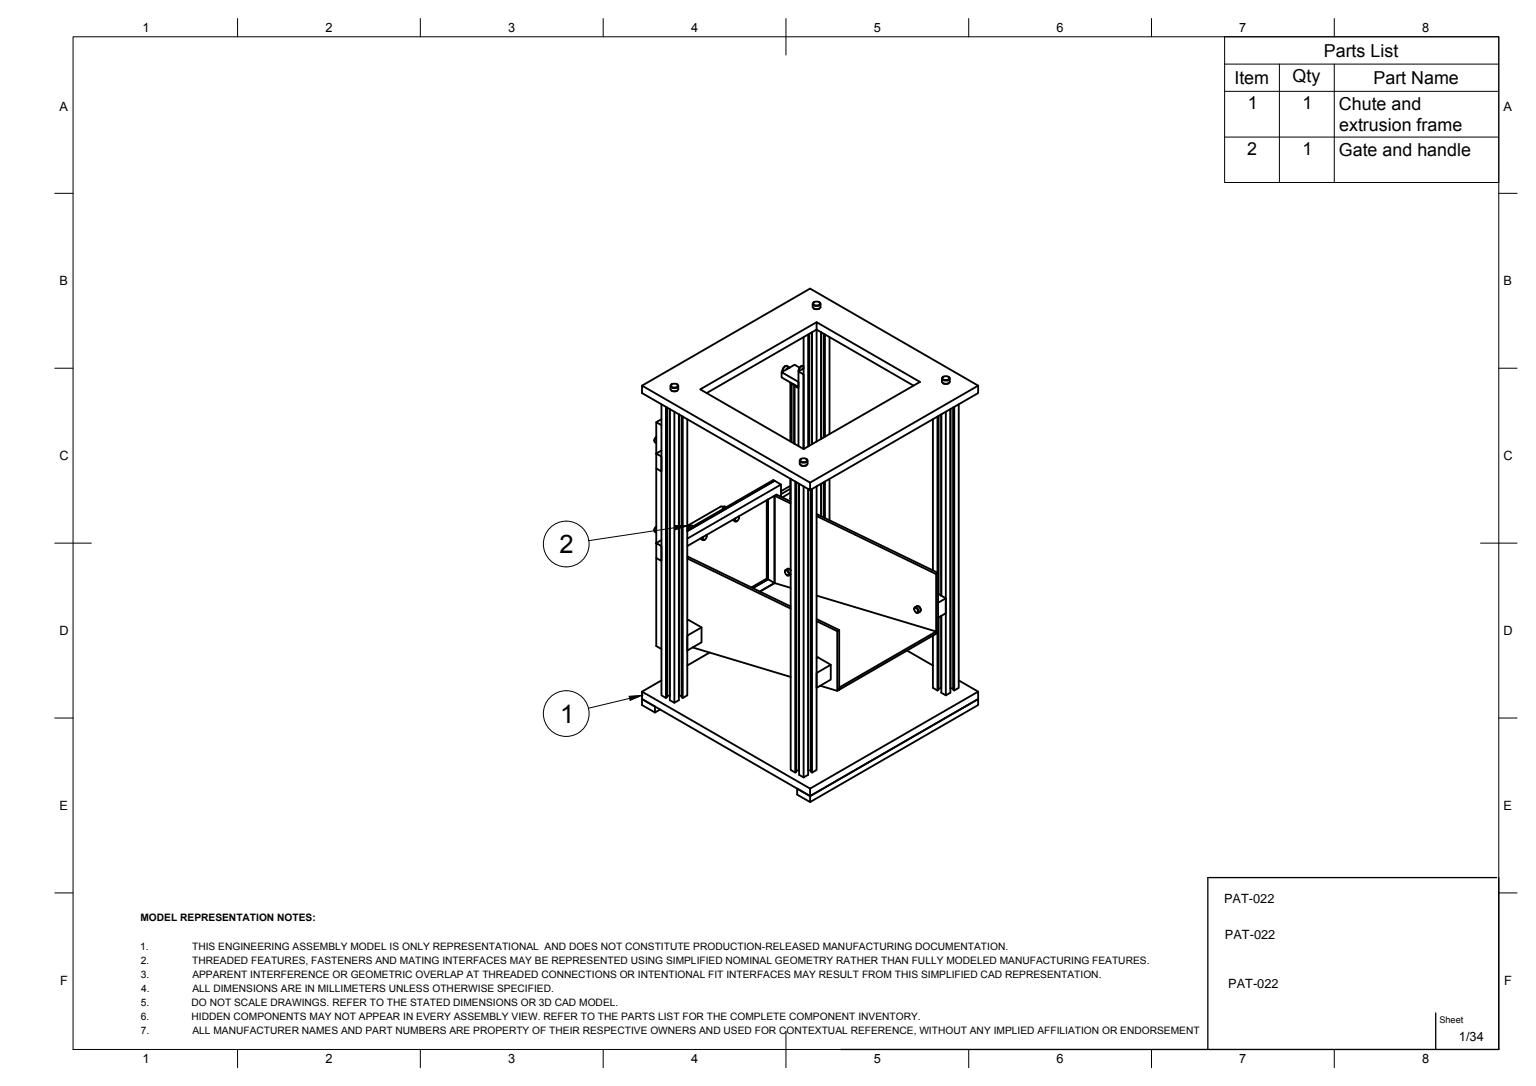
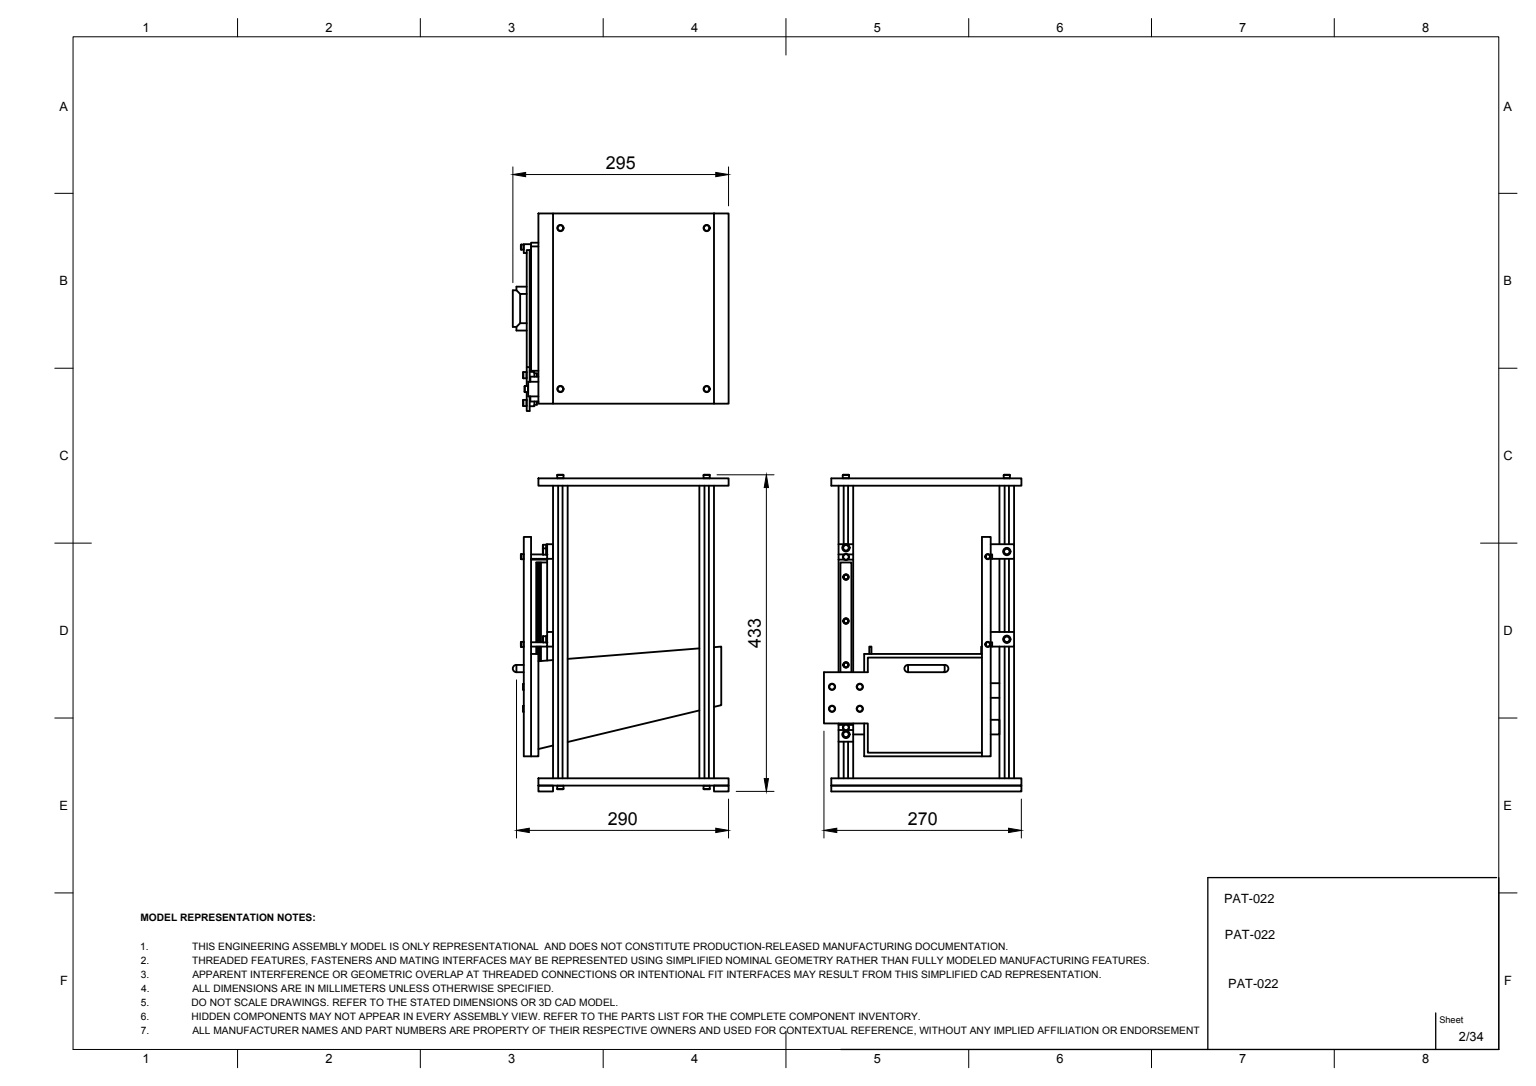
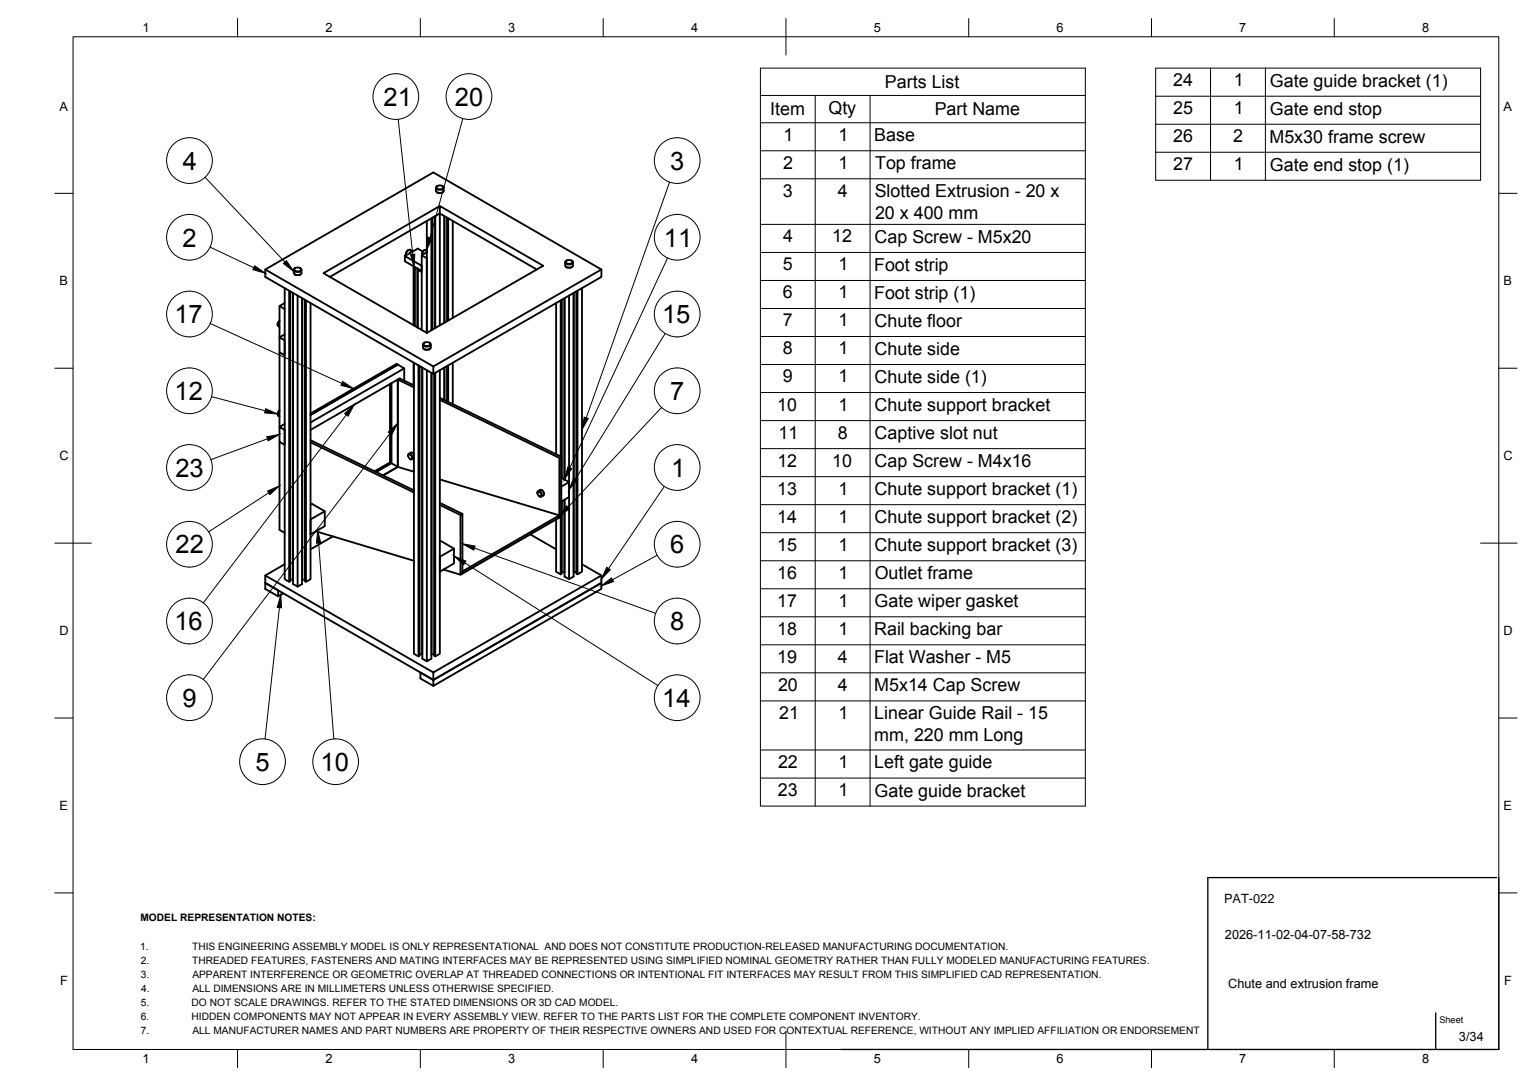
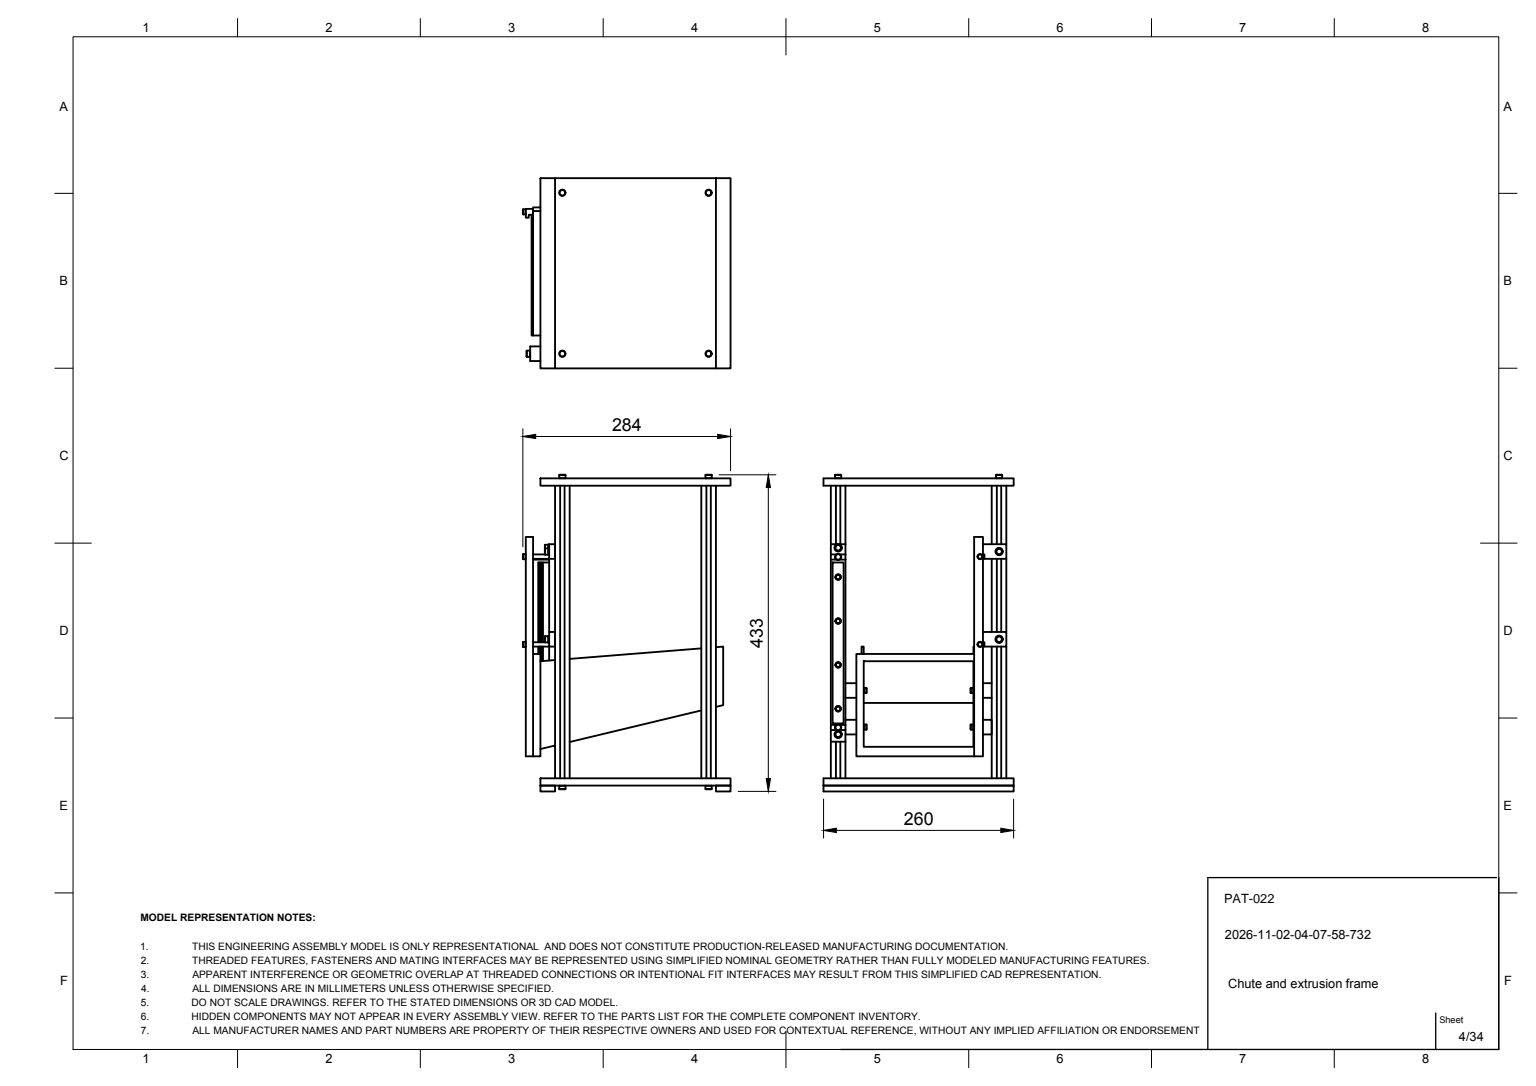
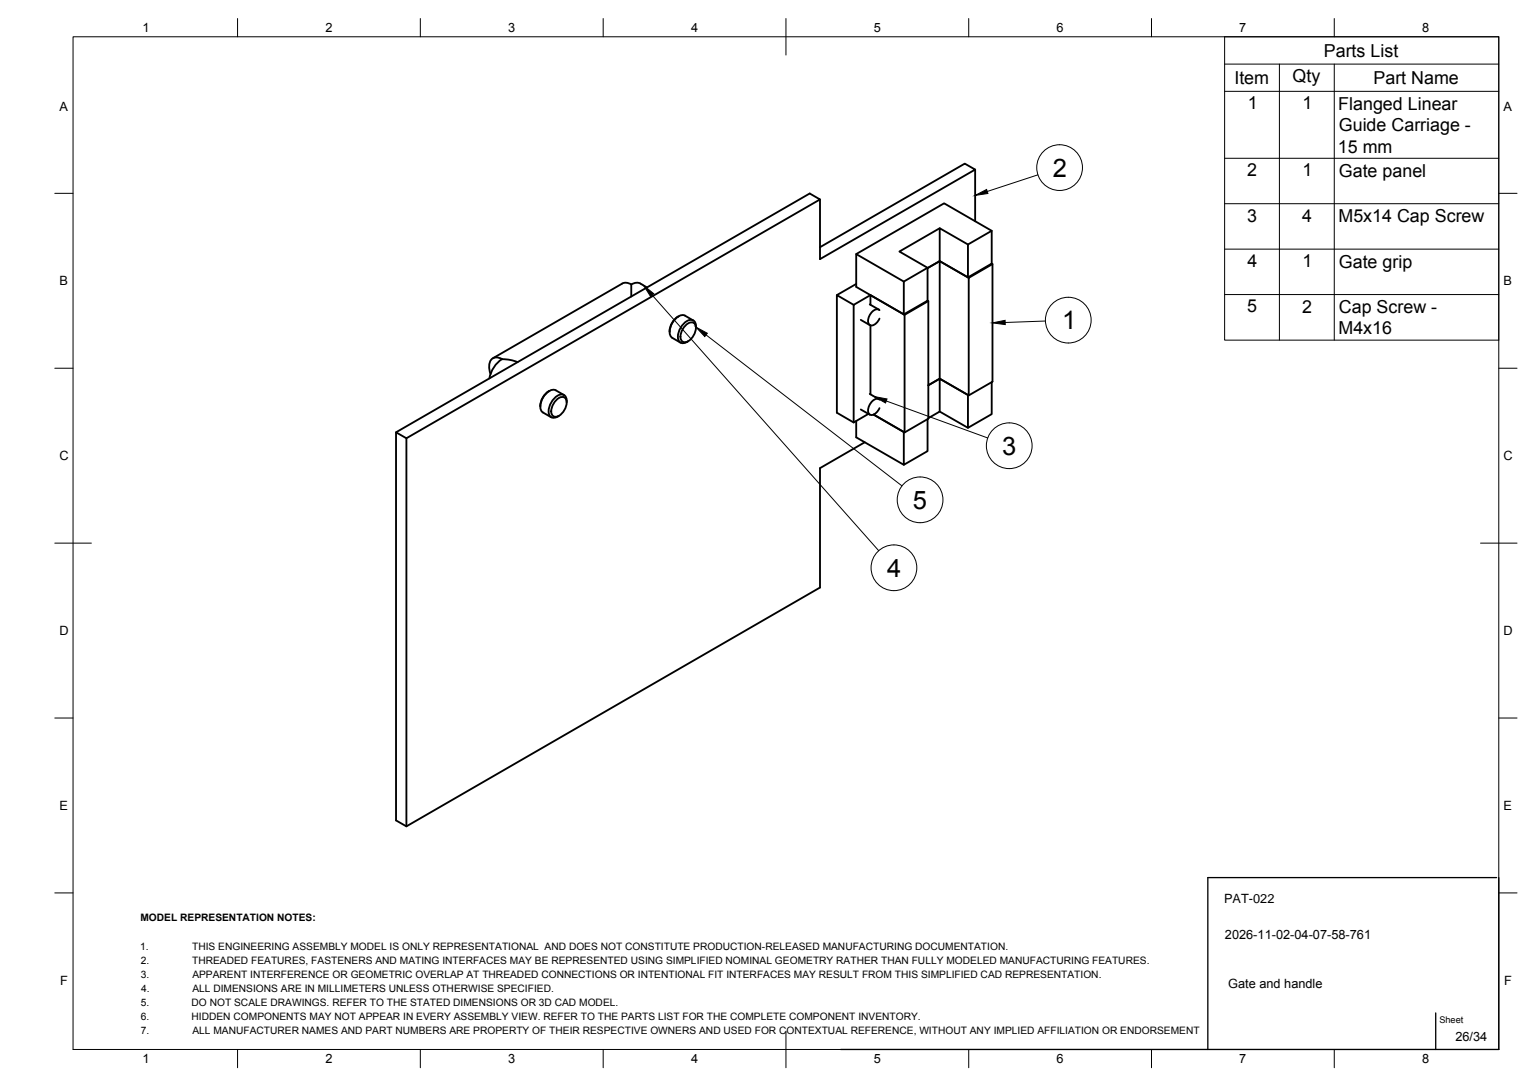
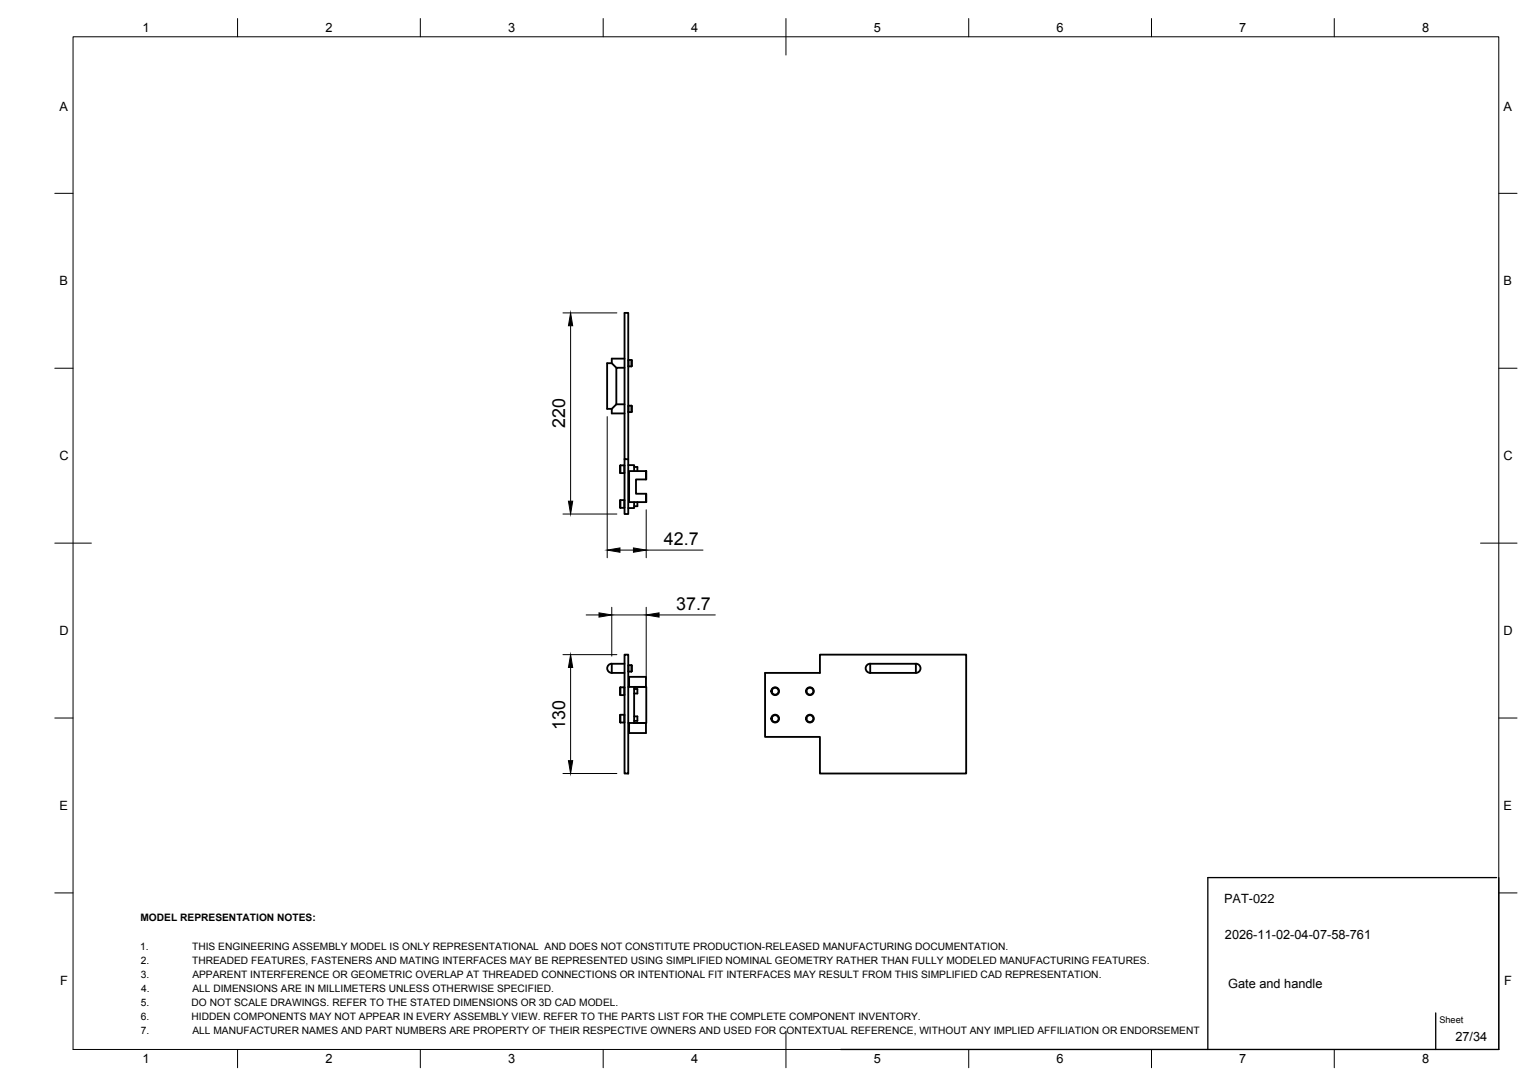
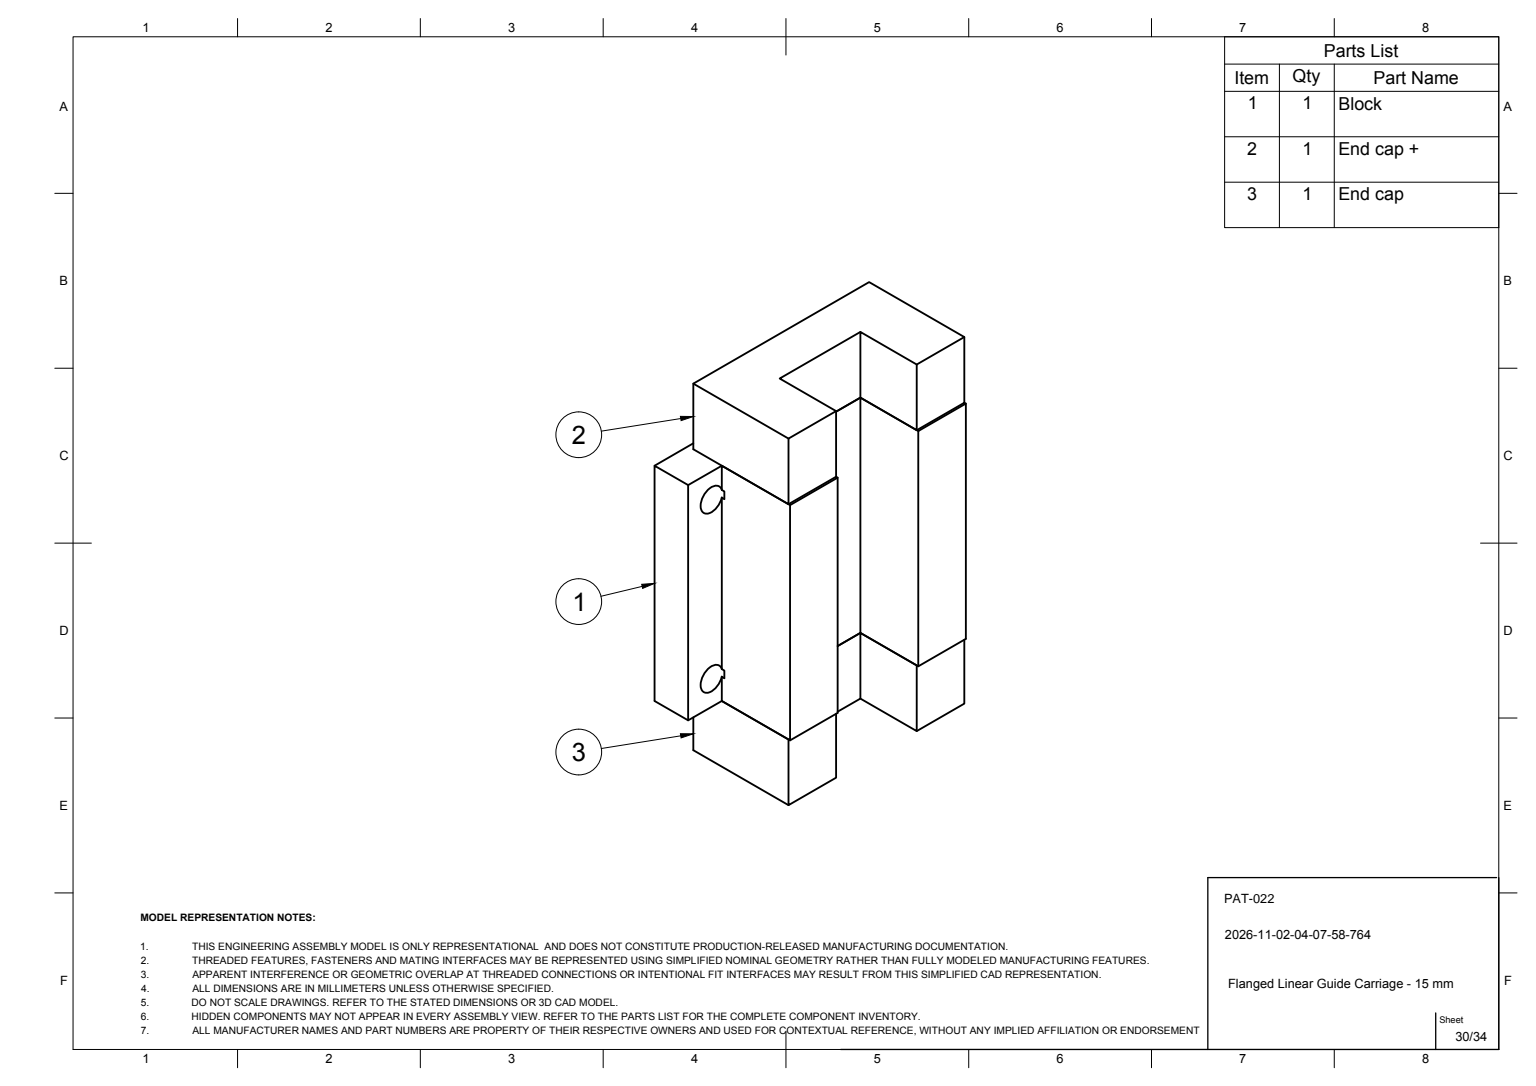
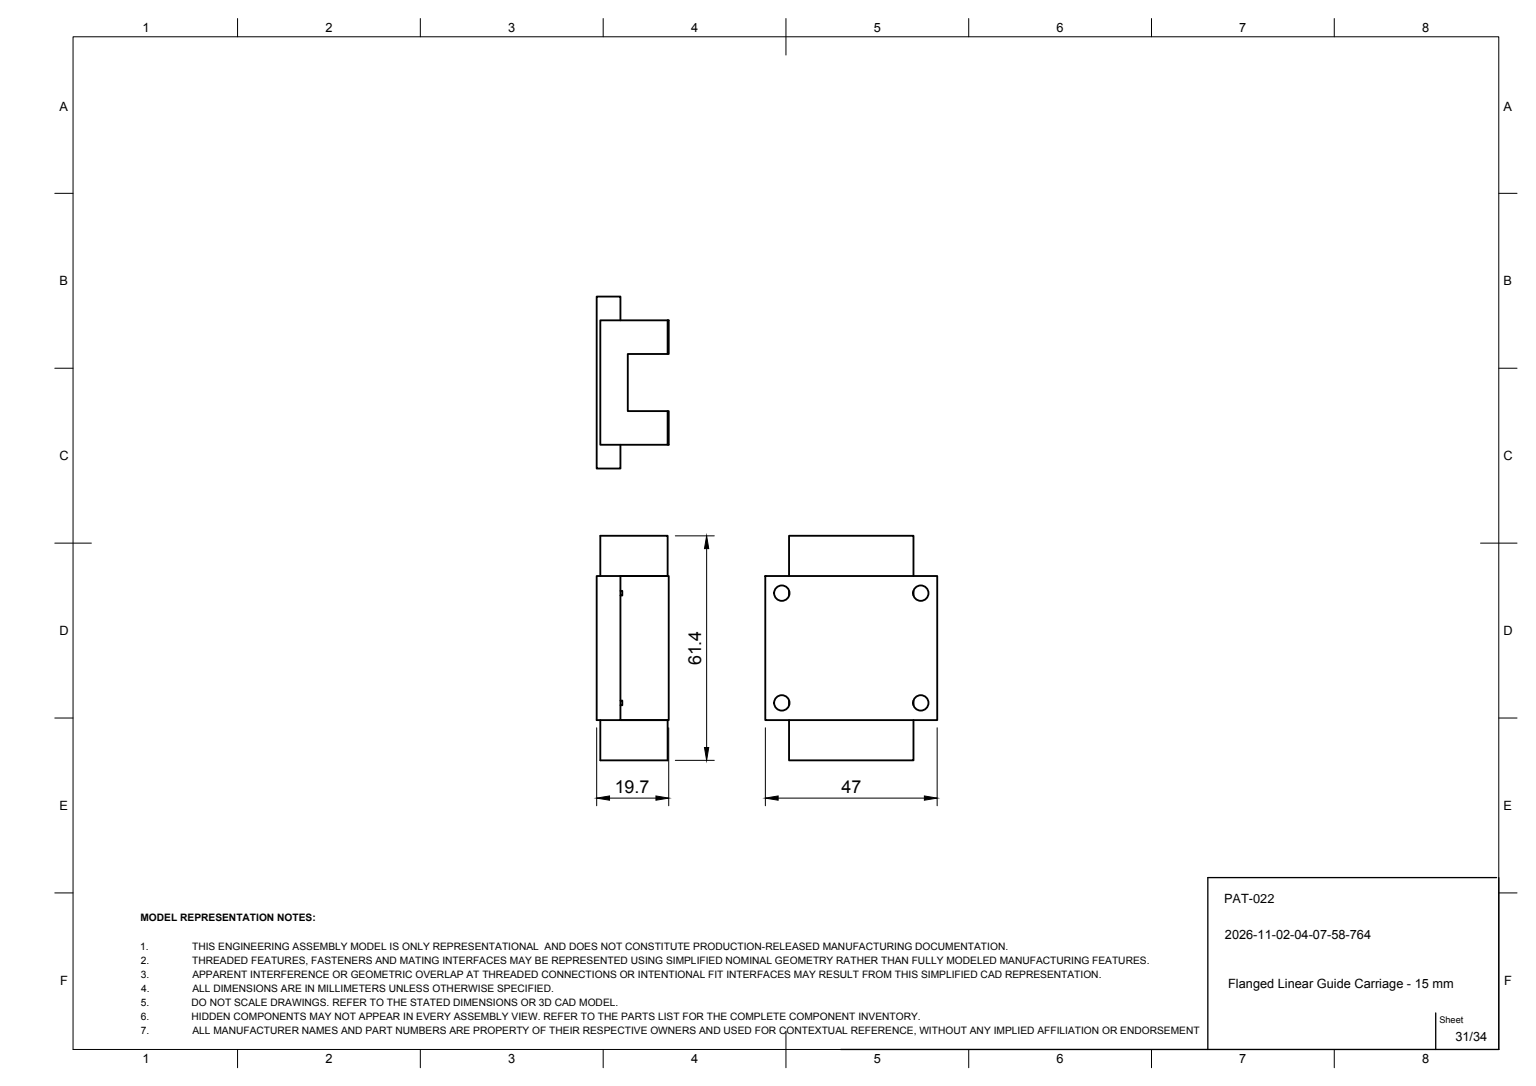
ISO-10303-21;
HEADER;
/* Generated by software containing ST-Developer
 * from STEP Tools, Inc. (www.steptools.com) 
 */

FILE_DESCRIPTION(
/* description */ ('Chute with adjustable gate'),
/* implementation_level */ '2;1');

FILE_NAME(
/* name */ 'PAT-022',
/* time_stamp */ '2026-10-27T10:52:28-07:00',
/* author */ (''),
/* organization */ (''),
/* preprocessor_version */ 'ST-DEVELOPER v20.2',
/* originating_system */ 'Autodesk Translation Framework v15.17.0.0',
/* authorisation */ '');

FILE_SCHEMA (('AUTOMOTIVE_DESIGN { 1 0 10303 214 3 1 1 }'));
ENDSEC;

DATA;
#10=MECHANICAL_DESIGN_GEOMETRIC_PRESENTATION_REPRESENTATION('',(#414,#415,
#416,#417,#418,#419,#420,#421,#422,#423,#424,#425,#426,#427,#428,#429,#430,
#431,#432,#433,#434,#435,#436,#437,#438,#439,#440,#441,#442,#443,#444,#445),
#13094);
#11=ITEM_DEFINED_TRANSFORMATION($,$,#8509,#8570);
#12=ITEM_DEFINED_TRANSFORMATION($,$,#8548,#8571);
#13=ITEM_DEFINED_TRANSFORMATION($,$,#8559,#8572);
#14=ITEM_DEFINED_TRANSFORMATION($,$,#7988,#8623);
#15=ITEM_DEFINED_TRANSFORMATION($,$,#8007,#8624);
#16=ITEM_DEFINED_TRANSFORMATION($,$,#8030,#8625);
#17=ITEM_DEFINED_TRANSFORMATION($,$,#8037,#8626);
#18=ITEM_DEFINED_TRANSFORMATION($,$,#8044,#8627);
#19=ITEM_DEFINED_TRANSFORMATION($,$,#8051,#8628);
#20=ITEM_DEFINED_TRANSFORMATION($,$,#8064,#8629);
#21=ITEM_DEFINED_TRANSFORMATION($,$,#8077,#8630);
#22=ITEM_DEFINED_TRANSFORMATION($,$,#8095,#8631);
#23=ITEM_DEFINED_TRANSFORMATION($,$,#8113,#8632);
#24=ITEM_DEFINED_TRANSFORMATION($,$,#8131,#8633);
#25=ITEM_DEFINED_TRANSFORMATION($,$,#8149,#8634);
#26=ITEM_DEFINED_TRANSFORMATION($,$,#8160,#8635);
#27=ITEM_DEFINED_TRANSFORMATION($,$,#8171,#8636);
#28=ITEM_DEFINED_TRANSFORMATION($,$,#8202,#8637);
#29=ITEM_DEFINED_TRANSFORMATION($,$,#8217,#8638);
#30=ITEM_DEFINED_TRANSFORMATION($,$,#8234,#8639);
#31=ITEM_DEFINED_TRANSFORMATION($,$,#8251,#8640);
#32=ITEM_DEFINED_TRANSFORMATION($,$,#8261,#8641);
#33=ITEM_DEFINED_TRANSFORMATION($,$,#8271,#8642);
#34=ITEM_DEFINED_TRANSFORMATION($,$,#8321,#8643);
#35=ITEM_DEFINED_TRANSFORMATION($,$,#8321,#8644);
#36=ITEM_DEFINED_TRANSFORMATION($,$,#8271,#8645);
#37=ITEM_DEFINED_TRANSFORMATION($,$,#8321,#8646);
#38=ITEM_DEFINED_TRANSFORMATION($,$,#8321,#8647);
#39=ITEM_DEFINED_TRANSFORMATION($,$,#8271,#8648);
#40=ITEM_DEFINED_TRANSFORMATION($,$,#8321,#8649);
#41=ITEM_DEFINED_TRANSFORMATION($,$,#8321,#8650);
#42=ITEM_DEFINED_TRANSFORMATION($,$,#8271,#8651);
#43=ITEM_DEFINED_TRANSFORMATION($,$,#8321,#8652);
#44=ITEM_DEFINED_TRANSFORMATION($,$,#8321,#8653);
#45=ITEM_DEFINED_TRANSFORMATION($,$,#8390,#8654);
#46=ITEM_DEFINED_TRANSFORMATION($,$,#8321,#8655);
#47=ITEM_DEFINED_TRANSFORMATION($,$,#8597,#8656);
#48=ITEM_DEFINED_TRANSFORMATION($,$,#8390,#8657);
#49=ITEM_DEFINED_TRANSFORMATION($,$,#8321,#8658);
#50=ITEM_DEFINED_TRANSFORMATION($,$,#8597,#8659);
#51=ITEM_DEFINED_TRANSFORMATION($,$,#8390,#8660);
#52=ITEM_DEFINED_TRANSFORMATION($,$,#8321,#8661);
#53=ITEM_DEFINED_TRANSFORMATION($,$,#8597,#8662);
#54=ITEM_DEFINED_TRANSFORMATION($,$,#8390,#8663);
#55=ITEM_DEFINED_TRANSFORMATION($,$,#8321,#8664);
#56=ITEM_DEFINED_TRANSFORMATION($,$,#8597,#8665);
#57=ITEM_DEFINED_TRANSFORMATION($,$,#8390,#8666);
#58=ITEM_DEFINED_TRANSFORMATION($,$,#8411,#8667);
#59=ITEM_DEFINED_TRANSFORMATION($,$,#8573,#8668);
#60=ITEM_DEFINED_TRANSFORMATION($,$,#8390,#8669);
#61=ITEM_DEFINED_TRANSFORMATION($,$,#8411,#8670);
#62=ITEM_DEFINED_TRANSFORMATION($,$,#8573,#8671);
#63=ITEM_DEFINED_TRANSFORMATION($,$,#8347,#8672);
#64=ITEM_DEFINED_TRANSFORMATION($,$,#8597,#8673);
#65=ITEM_DEFINED_TRANSFORMATION($,$,#8597,#8674);
#66=ITEM_DEFINED_TRANSFORMATION($,$,#8597,#8675);
#67=ITEM_DEFINED_TRANSFORMATION($,$,#8597,#8676);
#68=ITEM_DEFINED_TRANSFORMATION($,$,#8390,#8677);
#69=ITEM_DEFINED_TRANSFORMATION($,$,#8411,#8678);
#70=ITEM_DEFINED_TRANSFORMATION($,$,#8573,#8679);
#71=ITEM_DEFINED_TRANSFORMATION($,$,#8597,#8680);
#72=ITEM_DEFINED_TRANSFORMATION($,$,#8390,#8681);
#73=ITEM_DEFINED_TRANSFORMATION($,$,#8411,#8682);
#74=ITEM_DEFINED_TRANSFORMATION($,$,#8573,#8683);
#75=ITEM_DEFINED_TRANSFORMATION($,$,#8597,#8684);
#76=ITEM_DEFINED_TRANSFORMATION($,$,#8422,#8685);
#77=ITEM_DEFINED_TRANSFORMATION($,$,#8422,#8686);
#78=ITEM_DEFINED_TRANSFORMATION($,$,#8451,#8687);
#79=ITEM_DEFINED_TRANSFORMATION($,$,#8480,#8688);
#80=ITEM_DEFINED_TRANSFORMATION($,$,#8508,#8689);
#81=ITEM_DEFINED_TRANSFORMATION($,$,#8573,#8690);
#82=ITEM_DEFINED_TRANSFORMATION($,$,#8573,#8691);
#83=ITEM_DEFINED_TRANSFORMATION($,$,#8573,#8692);
#84=ITEM_DEFINED_TRANSFORMATION($,$,#8573,#8693);
#85=ITEM_DEFINED_TRANSFORMATION($,$,#8597,#8694);
#86=ITEM_DEFINED_TRANSFORMATION($,$,#8597,#8695);
#87=ITEM_DEFINED_TRANSFORMATION($,$,#7987,#8696);
#88=ITEM_DEFINED_TRANSFORMATION($,$,#8450,#8697);
#89=(
REPRESENTATION_RELATIONSHIP($,$,#13280,#13279)
REPRESENTATION_RELATIONSHIP_WITH_TRANSFORMATION(#11)
SHAPE_REPRESENTATION_RELATIONSHIP()
);
#90=(
REPRESENTATION_RELATIONSHIP($,$,#13281,#13279)
REPRESENTATION_RELATIONSHIP_WITH_TRANSFORMATION(#12)
SHAPE_REPRESENTATION_RELATIONSHIP()
);
#91=(
REPRESENTATION_RELATIONSHIP($,$,#13282,#13279)
REPRESENTATION_RELATIONSHIP_WITH_TRANSFORMATION(#13)
SHAPE_REPRESENTATION_RELATIONSHIP()
);
#92=(
REPRESENTATION_RELATIONSHIP($,$,#13251,#13250)
REPRESENTATION_RELATIONSHIP_WITH_TRANSFORMATION(#14)
SHAPE_REPRESENTATION_RELATIONSHIP()
);
#93=(
REPRESENTATION_RELATIONSHIP($,$,#13252,#13250)
REPRESENTATION_RELATIONSHIP_WITH_TRANSFORMATION(#15)
SHAPE_REPRESENTATION_RELATIONSHIP()
);
#94=(
REPRESENTATION_RELATIONSHIP($,$,#13253,#13250)
REPRESENTATION_RELATIONSHIP_WITH_TRANSFORMATION(#16)
SHAPE_REPRESENTATION_RELATIONSHIP()
);
#95=(
REPRESENTATION_RELATIONSHIP($,$,#13254,#13250)
REPRESENTATION_RELATIONSHIP_WITH_TRANSFORMATION(#17)
SHAPE_REPRESENTATION_RELATIONSHIP()
);
#96=(
REPRESENTATION_RELATIONSHIP($,$,#13255,#13250)
REPRESENTATION_RELATIONSHIP_WITH_TRANSFORMATION(#18)
SHAPE_REPRESENTATION_RELATIONSHIP()
);
#97=(
REPRESENTATION_RELATIONSHIP($,$,#13256,#13250)
REPRESENTATION_RELATIONSHIP_WITH_TRANSFORMATION(#19)
SHAPE_REPRESENTATION_RELATIONSHIP()
);
#98=(
REPRESENTATION_RELATIONSHIP($,$,#13257,#13250)
REPRESENTATION_RELATIONSHIP_WITH_TRANSFORMATION(#20)
SHAPE_REPRESENTATION_RELATIONSHIP()
);
#99=(
REPRESENTATION_RELATIONSHIP($,$,#13258,#13250)
REPRESENTATION_RELATIONSHIP_WITH_TRANSFORMATION(#21)
SHAPE_REPRESENTATION_RELATIONSHIP()
);
#100=(
REPRESENTATION_RELATIONSHIP($,$,#13259,#13250)
REPRESENTATION_RELATIONSHIP_WITH_TRANSFORMATION(#22)
SHAPE_REPRESENTATION_RELATIONSHIP()
);
#101=(
REPRESENTATION_RELATIONSHIP($,$,#13260,#13250)
REPRESENTATION_RELATIONSHIP_WITH_TRANSFORMATION(#23)
SHAPE_REPRESENTATION_RELATIONSHIP()
);
#102=(
REPRESENTATION_RELATIONSHIP($,$,#13261,#13250)
REPRESENTATION_RELATIONSHIP_WITH_TRANSFORMATION(#24)
SHAPE_REPRESENTATION_RELATIONSHIP()
);
#103=(
REPRESENTATION_RELATIONSHIP($,$,#13262,#13250)
REPRESENTATION_RELATIONSHIP_WITH_TRANSFORMATION(#25)
SHAPE_REPRESENTATION_RELATIONSHIP()
);
#104=(
REPRESENTATION_RELATIONSHIP($,$,#13263,#13250)
REPRESENTATION_RELATIONSHIP_WITH_TRANSFORMATION(#26)
SHAPE_REPRESENTATION_RELATIONSHIP()
);
#105=(
REPRESENTATION_RELATIONSHIP($,$,#13264,#13250)
REPRESENTATION_RELATIONSHIP_WITH_TRANSFORMATION(#27)
SHAPE_REPRESENTATION_RELATIONSHIP()
);
#106=(
REPRESENTATION_RELATIONSHIP($,$,#13265,#13250)
REPRESENTATION_RELATIONSHIP_WITH_TRANSFORMATION(#28)
SHAPE_REPRESENTATION_RELATIONSHIP()
);
#107=(
REPRESENTATION_RELATIONSHIP($,$,#13266,#13250)
REPRESENTATION_RELATIONSHIP_WITH_TRANSFORMATION(#29)
SHAPE_REPRESENTATION_RELATIONSHIP()
);
#108=(
REPRESENTATION_RELATIONSHIP($,$,#13267,#13250)
REPRESENTATION_RELATIONSHIP_WITH_TRANSFORMATION(#30)
SHAPE_REPRESENTATION_RELATIONSHIP()
);
#109=(
REPRESENTATION_RELATIONSHIP($,$,#13268,#13250)
REPRESENTATION_RELATIONSHIP_WITH_TRANSFORMATION(#31)
SHAPE_REPRESENTATION_RELATIONSHIP()
);
#110=(
REPRESENTATION_RELATIONSHIP($,$,#13269,#13250)
REPRESENTATION_RELATIONSHIP_WITH_TRANSFORMATION(#32)
SHAPE_REPRESENTATION_RELATIONSHIP()
);
#111=(
REPRESENTATION_RELATIONSHIP($,$,#13270,#13250)
REPRESENTATION_RELATIONSHIP_WITH_TRANSFORMATION(#33)
SHAPE_REPRESENTATION_RELATIONSHIP()
);
#112=(
REPRESENTATION_RELATIONSHIP($,$,#13271,#13250)
REPRESENTATION_RELATIONSHIP_WITH_TRANSFORMATION(#34)
SHAPE_REPRESENTATION_RELATIONSHIP()
);
#113=(
REPRESENTATION_RELATIONSHIP($,$,#13271,#13250)
REPRESENTATION_RELATIONSHIP_WITH_TRANSFORMATION(#35)
SHAPE_REPRESENTATION_RELATIONSHIP()
);
#114=(
REPRESENTATION_RELATIONSHIP($,$,#13270,#13250)
REPRESENTATION_RELATIONSHIP_WITH_TRANSFORMATION(#36)
SHAPE_REPRESENTATION_RELATIONSHIP()
);
#115=(
REPRESENTATION_RELATIONSHIP($,$,#13271,#13250)
REPRESENTATION_RELATIONSHIP_WITH_TRANSFORMATION(#37)
SHAPE_REPRESENTATION_RELATIONSHIP()
);
#116=(
REPRESENTATION_RELATIONSHIP($,$,#13271,#13250)
REPRESENTATION_RELATIONSHIP_WITH_TRANSFORMATION(#38)
SHAPE_REPRESENTATION_RELATIONSHIP()
);
#117=(
REPRESENTATION_RELATIONSHIP($,$,#13270,#13250)
REPRESENTATION_RELATIONSHIP_WITH_TRANSFORMATION(#39)
SHAPE_REPRESENTATION_RELATIONSHIP()
);
#118=(
REPRESENTATION_RELATIONSHIP($,$,#13271,#13250)
REPRESENTATION_RELATIONSHIP_WITH_TRANSFORMATION(#40)
SHAPE_REPRESENTATION_RELATIONSHIP()
);
#119=(
REPRESENTATION_RELATIONSHIP($,$,#13271,#13250)
REPRESENTATION_RELATIONSHIP_WITH_TRANSFORMATION(#41)
SHAPE_REPRESENTATION_RELATIONSHIP()
);
#120=(
REPRESENTATION_RELATIONSHIP($,$,#13270,#13250)
REPRESENTATION_RELATIONSHIP_WITH_TRANSFORMATION(#42)
SHAPE_REPRESENTATION_RELATIONSHIP()
);
#121=(
REPRESENTATION_RELATIONSHIP($,$,#13271,#13250)
REPRESENTATION_RELATIONSHIP_WITH_TRANSFORMATION(#43)
SHAPE_REPRESENTATION_RELATIONSHIP()
);
#122=(
REPRESENTATION_RELATIONSHIP($,$,#13271,#13250)
REPRESENTATION_RELATIONSHIP_WITH_TRANSFORMATION(#44)
SHAPE_REPRESENTATION_RELATIONSHIP()
);
#123=(
REPRESENTATION_RELATIONSHIP($,$,#13273,#13250)
REPRESENTATION_RELATIONSHIP_WITH_TRANSFORMATION(#45)
SHAPE_REPRESENTATION_RELATIONSHIP()
);
#124=(
REPRESENTATION_RELATIONSHIP($,$,#13271,#13250)
REPRESENTATION_RELATIONSHIP_WITH_TRANSFORMATION(#46)
SHAPE_REPRESENTATION_RELATIONSHIP()
);
#125=(
REPRESENTATION_RELATIONSHIP($,$,#13284,#13250)
REPRESENTATION_RELATIONSHIP_WITH_TRANSFORMATION(#47)
SHAPE_REPRESENTATION_RELATIONSHIP()
);
#126=(
REPRESENTATION_RELATIONSHIP($,$,#13273,#13250)
REPRESENTATION_RELATIONSHIP_WITH_TRANSFORMATION(#48)
SHAPE_REPRESENTATION_RELATIONSHIP()
);
#127=(
REPRESENTATION_RELATIONSHIP($,$,#13271,#13250)
REPRESENTATION_RELATIONSHIP_WITH_TRANSFORMATION(#49)
SHAPE_REPRESENTATION_RELATIONSHIP()
);
#128=(
REPRESENTATION_RELATIONSHIP($,$,#13284,#13250)
REPRESENTATION_RELATIONSHIP_WITH_TRANSFORMATION(#50)
SHAPE_REPRESENTATION_RELATIONSHIP()
);
#129=(
REPRESENTATION_RELATIONSHIP($,$,#13273,#13250)
REPRESENTATION_RELATIONSHIP_WITH_TRANSFORMATION(#51)
SHAPE_REPRESENTATION_RELATIONSHIP()
);
#130=(
REPRESENTATION_RELATIONSHIP($,$,#13271,#13250)
REPRESENTATION_RELATIONSHIP_WITH_TRANSFORMATION(#52)
SHAPE_REPRESENTATION_RELATIONSHIP()
);
#131=(
REPRESENTATION_RELATIONSHIP($,$,#13284,#13250)
REPRESENTATION_RELATIONSHIP_WITH_TRANSFORMATION(#53)
SHAPE_REPRESENTATION_RELATIONSHIP()
);
#132=(
REPRESENTATION_RELATIONSHIP($,$,#13273,#13250)
REPRESENTATION_RELATIONSHIP_WITH_TRANSFORMATION(#54)
SHAPE_REPRESENTATION_RELATIONSHIP()
);
#133=(
REPRESENTATION_RELATIONSHIP($,$,#13271,#13250)
REPRESENTATION_RELATIONSHIP_WITH_TRANSFORMATION(#55)
SHAPE_REPRESENTATION_RELATIONSHIP()
);
#134=(
REPRESENTATION_RELATIONSHIP($,$,#13284,#13250)
REPRESENTATION_RELATIONSHIP_WITH_TRANSFORMATION(#56)
SHAPE_REPRESENTATION_RELATIONSHIP()
);
#135=(
REPRESENTATION_RELATIONSHIP($,$,#13273,#13250)
REPRESENTATION_RELATIONSHIP_WITH_TRANSFORMATION(#57)
SHAPE_REPRESENTATION_RELATIONSHIP()
);
#136=(
REPRESENTATION_RELATIONSHIP($,$,#13274,#13250)
REPRESENTATION_RELATIONSHIP_WITH_TRANSFORMATION(#58)
SHAPE_REPRESENTATION_RELATIONSHIP()
);
#137=(
REPRESENTATION_RELATIONSHIP($,$,#13283,#13250)
REPRESENTATION_RELATIONSHIP_WITH_TRANSFORMATION(#59)
SHAPE_REPRESENTATION_RELATIONSHIP()
);
#138=(
REPRESENTATION_RELATIONSHIP($,$,#13273,#13250)
REPRESENTATION_RELATIONSHIP_WITH_TRANSFORMATION(#60)
SHAPE_REPRESENTATION_RELATIONSHIP()
);
#139=(
REPRESENTATION_RELATIONSHIP($,$,#13274,#13250)
REPRESENTATION_RELATIONSHIP_WITH_TRANSFORMATION(#61)
SHAPE_REPRESENTATION_RELATIONSHIP()
);
#140=(
REPRESENTATION_RELATIONSHIP($,$,#13283,#13250)
REPRESENTATION_RELATIONSHIP_WITH_TRANSFORMATION(#62)
SHAPE_REPRESENTATION_RELATIONSHIP()
);
#141=(
REPRESENTATION_RELATIONSHIP($,$,#13272,#13250)
REPRESENTATION_RELATIONSHIP_WITH_TRANSFORMATION(#63)
SHAPE_REPRESENTATION_RELATIONSHIP()
);
#142=(
REPRESENTATION_RELATIONSHIP($,$,#13284,#13250)
REPRESENTATION_RELATIONSHIP_WITH_TRANSFORMATION(#64)
SHAPE_REPRESENTATION_RELATIONSHIP()
);
#143=(
REPRESENTATION_RELATIONSHIP($,$,#13284,#13250)
REPRESENTATION_RELATIONSHIP_WITH_TRANSFORMATION(#65)
SHAPE_REPRESENTATION_RELATIONSHIP()
);
#144=(
REPRESENTATION_RELATIONSHIP($,$,#13284,#13250)
REPRESENTATION_RELATIONSHIP_WITH_TRANSFORMATION(#66)
SHAPE_REPRESENTATION_RELATIONSHIP()
);
#145=(
REPRESENTATION_RELATIONSHIP($,$,#13284,#13250)
REPRESENTATION_RELATIONSHIP_WITH_TRANSFORMATION(#67)
SHAPE_REPRESENTATION_RELATIONSHIP()
);
#146=(
REPRESENTATION_RELATIONSHIP($,$,#13273,#13250)
REPRESENTATION_RELATIONSHIP_WITH_TRANSFORMATION(#68)
SHAPE_REPRESENTATION_RELATIONSHIP()
);
#147=(
REPRESENTATION_RELATIONSHIP($,$,#13274,#13250)
REPRESENTATION_RELATIONSHIP_WITH_TRANSFORMATION(#69)
SHAPE_REPRESENTATION_RELATIONSHIP()
);
#148=(
REPRESENTATION_RELATIONSHIP($,$,#13283,#13250)
REPRESENTATION_RELATIONSHIP_WITH_TRANSFORMATION(#70)
SHAPE_REPRESENTATION_RELATIONSHIP()
);
#149=(
REPRESENTATION_RELATIONSHIP($,$,#13284,#13250)
REPRESENTATION_RELATIONSHIP_WITH_TRANSFORMATION(#71)
SHAPE_REPRESENTATION_RELATIONSHIP()
);
#150=(
REPRESENTATION_RELATIONSHIP($,$,#13273,#13250)
REPRESENTATION_RELATIONSHIP_WITH_TRANSFORMATION(#72)
SHAPE_REPRESENTATION_RELATIONSHIP()
);
#151=(
REPRESENTATION_RELATIONSHIP($,$,#13274,#13250)
REPRESENTATION_RELATIONSHIP_WITH_TRANSFORMATION(#73)
SHAPE_REPRESENTATION_RELATIONSHIP()
);
#152=(
REPRESENTATION_RELATIONSHIP($,$,#13283,#13250)
REPRESENTATION_RELATIONSHIP_WITH_TRANSFORMATION(#74)
SHAPE_REPRESENTATION_RELATIONSHIP()
);
#153=(
REPRESENTATION_RELATIONSHIP($,$,#13284,#13250)
REPRESENTATION_RELATIONSHIP_WITH_TRANSFORMATION(#75)
SHAPE_REPRESENTATION_RELATIONSHIP()
);
#154=(
REPRESENTATION_RELATIONSHIP($,$,#13275,#13250)
REPRESENTATION_RELATIONSHIP_WITH_TRANSFORMATION(#76)
SHAPE_REPRESENTATION_RELATIONSHIP()
);
#155=(
REPRESENTATION_RELATIONSHIP($,$,#13275,#13250)
REPRESENTATION_RELATIONSHIP_WITH_TRANSFORMATION(#77)
SHAPE_REPRESENTATION_RELATIONSHIP()
);
#156=(
REPRESENTATION_RELATIONSHIP($,$,#13277,#13276)
REPRESENTATION_RELATIONSHIP_WITH_TRANSFORMATION(#78)
SHAPE_REPRESENTATION_RELATIONSHIP()
);
#157=(
REPRESENTATION_RELATIONSHIP($,$,#13278,#13276)
REPRESENTATION_RELATIONSHIP_WITH_TRANSFORMATION(#79)
SHAPE_REPRESENTATION_RELATIONSHIP()
);
#158=(
REPRESENTATION_RELATIONSHIP($,$,#13279,#13276)
REPRESENTATION_RELATIONSHIP_WITH_TRANSFORMATION(#80)
SHAPE_REPRESENTATION_RELATIONSHIP()
);
#159=(
REPRESENTATION_RELATIONSHIP($,$,#13283,#13276)
REPRESENTATION_RELATIONSHIP_WITH_TRANSFORMATION(#81)
SHAPE_REPRESENTATION_RELATIONSHIP()
);
#160=(
REPRESENTATION_RELATIONSHIP($,$,#13283,#13276)
REPRESENTATION_RELATIONSHIP_WITH_TRANSFORMATION(#82)
SHAPE_REPRESENTATION_RELATIONSHIP()
);
#161=(
REPRESENTATION_RELATIONSHIP($,$,#13283,#13276)
REPRESENTATION_RELATIONSHIP_WITH_TRANSFORMATION(#83)
SHAPE_REPRESENTATION_RELATIONSHIP()
);
#162=(
REPRESENTATION_RELATIONSHIP($,$,#13283,#13276)
REPRESENTATION_RELATIONSHIP_WITH_TRANSFORMATION(#84)
SHAPE_REPRESENTATION_RELATIONSHIP()
);
#163=(
REPRESENTATION_RELATIONSHIP($,$,#13284,#13276)
REPRESENTATION_RELATIONSHIP_WITH_TRANSFORMATION(#85)
SHAPE_REPRESENTATION_RELATIONSHIP()
);
#164=(
REPRESENTATION_RELATIONSHIP($,$,#13284,#13276)
REPRESENTATION_RELATIONSHIP_WITH_TRANSFORMATION(#86)
SHAPE_REPRESENTATION_RELATIONSHIP()
);
#165=(
REPRESENTATION_RELATIONSHIP($,$,#13250,#13249)
REPRESENTATION_RELATIONSHIP_WITH_TRANSFORMATION(#87)
SHAPE_REPRESENTATION_RELATIONSHIP()
);
#166=(
REPRESENTATION_RELATIONSHIP($,$,#13276,#13249)
REPRESENTATION_RELATIONSHIP_WITH_TRANSFORMATION(#88)
SHAPE_REPRESENTATION_RELATIONSHIP()
);
#167=CONTEXT_DEPENDENT_SHAPE_REPRESENTATION(#89,#13169);
#168=CONTEXT_DEPENDENT_SHAPE_REPRESENTATION(#90,#13170);
#169=CONTEXT_DEPENDENT_SHAPE_REPRESENTATION(#91,#13171);
#170=CONTEXT_DEPENDENT_SHAPE_REPRESENTATION(#92,#13174);
#171=CONTEXT_DEPENDENT_SHAPE_REPRESENTATION(#93,#13175);
#172=CONTEXT_DEPENDENT_SHAPE_REPRESENTATION(#94,#13176);
#173=CONTEXT_DEPENDENT_SHAPE_REPRESENTATION(#95,#13177);
#174=CONTEXT_DEPENDENT_SHAPE_REPRESENTATION(#96,#13178);
#175=CONTEXT_DEPENDENT_SHAPE_REPRESENTATION(#97,#13179);
#176=CONTEXT_DEPENDENT_SHAPE_REPRESENTATION(#98,#13180);
#177=CONTEXT_DEPENDENT_SHAPE_REPRESENTATION(#99,#13181);
#178=CONTEXT_DEPENDENT_SHAPE_REPRESENTATION(#100,#13182);
#179=CONTEXT_DEPENDENT_SHAPE_REPRESENTATION(#101,#13183);
#180=CONTEXT_DEPENDENT_SHAPE_REPRESENTATION(#102,#13184);
#181=CONTEXT_DEPENDENT_SHAPE_REPRESENTATION(#103,#13185);
#182=CONTEXT_DEPENDENT_SHAPE_REPRESENTATION(#104,#13186);
#183=CONTEXT_DEPENDENT_SHAPE_REPRESENTATION(#105,#13187);
#184=CONTEXT_DEPENDENT_SHAPE_REPRESENTATION(#106,#13188);
#185=CONTEXT_DEPENDENT_SHAPE_REPRESENTATION(#107,#13189);
#186=CONTEXT_DEPENDENT_SHAPE_REPRESENTATION(#108,#13190);
#187=CONTEXT_DEPENDENT_SHAPE_REPRESENTATION(#109,#13191);
#188=CONTEXT_DEPENDENT_SHAPE_REPRESENTATION(#110,#13192);
#189=CONTEXT_DEPENDENT_SHAPE_REPRESENTATION(#111,#13193);
#190=CONTEXT_DEPENDENT_SHAPE_REPRESENTATION(#112,#13194);
#191=CONTEXT_DEPENDENT_SHAPE_REPRESENTATION(#113,#13195);
#192=CONTEXT_DEPENDENT_SHAPE_REPRESENTATION(#114,#13196);
#193=CONTEXT_DEPENDENT_SHAPE_REPRESENTATION(#115,#13197);
#194=CONTEXT_DEPENDENT_SHAPE_REPRESENTATION(#116,#13198);
#195=CONTEXT_DEPENDENT_SHAPE_REPRESENTATION(#117,#13199);
#196=CONTEXT_DEPENDENT_SHAPE_REPRESENTATION(#118,#13200);
#197=CONTEXT_DEPENDENT_SHAPE_REPRESENTATION(#119,#13201);
#198=CONTEXT_DEPENDENT_SHAPE_REPRESENTATION(#120,#13202);
#199=CONTEXT_DEPENDENT_SHAPE_REPRESENTATION(#121,#13203);
#200=CONTEXT_DEPENDENT_SHAPE_REPRESENTATION(#122,#13204);
#201=CONTEXT_DEPENDENT_SHAPE_REPRESENTATION(#123,#13205);
#202=CONTEXT_DEPENDENT_SHAPE_REPRESENTATION(#124,#13206);
#203=CONTEXT_DEPENDENT_SHAPE_REPRESENTATION(#125,#13207);
#204=CONTEXT_DEPENDENT_SHAPE_REPRESENTATION(#126,#13208);
#205=CONTEXT_DEPENDENT_SHAPE_REPRESENTATION(#127,#13209);
#206=CONTEXT_DEPENDENT_SHAPE_REPRESENTATION(#128,#13210);
#207=CONTEXT_DEPENDENT_SHAPE_REPRESENTATION(#129,#13211);
#208=CONTEXT_DEPENDENT_SHAPE_REPRESENTATION(#130,#13212);
#209=CONTEXT_DEPENDENT_SHAPE_REPRESENTATION(#131,#13213);
#210=CONTEXT_DEPENDENT_SHAPE_REPRESENTATION(#132,#13214);
#211=CONTEXT_DEPENDENT_SHAPE_REPRESENTATION(#133,#13215);
#212=CONTEXT_DEPENDENT_SHAPE_REPRESENTATION(#134,#13216);
#213=CONTEXT_DEPENDENT_SHAPE_REPRESENTATION(#135,#13217);
#214=CONTEXT_DEPENDENT_SHAPE_REPRESENTATION(#136,#13218);
#215=CONTEXT_DEPENDENT_SHAPE_REPRESENTATION(#137,#13219);
#216=CONTEXT_DEPENDENT_SHAPE_REPRESENTATION(#138,#13220);
#217=CONTEXT_DEPENDENT_SHAPE_REPRESENTATION(#139,#13221);
#218=CONTEXT_DEPENDENT_SHAPE_REPRESENTATION(#140,#13222);
#219=CONTEXT_DEPENDENT_SHAPE_REPRESENTATION(#141,#13223);
#220=CONTEXT_DEPENDENT_SHAPE_REPRESENTATION(#142,#13224);
#221=CONTEXT_DEPENDENT_SHAPE_REPRESENTATION(#143,#13225);
#222=CONTEXT_DEPENDENT_SHAPE_REPRESENTATION(#144,#13226);
#223=CONTEXT_DEPENDENT_SHAPE_REPRESENTATION(#145,#13227);
#224=CONTEXT_DEPENDENT_SHAPE_REPRESENTATION(#146,#13228);
#225=CONTEXT_DEPENDENT_SHAPE_REPRESENTATION(#147,#13229);
#226=CONTEXT_DEPENDENT_SHAPE_REPRESENTATION(#148,#13230);
#227=CONTEXT_DEPENDENT_SHAPE_REPRESENTATION(#149,#13231);
#228=CONTEXT_DEPENDENT_SHAPE_REPRESENTATION(#150,#13232);
#229=CONTEXT_DEPENDENT_SHAPE_REPRESENTATION(#151,#13233);
#230=CONTEXT_DEPENDENT_SHAPE_REPRESENTATION(#152,#13234);
#231=CONTEXT_DEPENDENT_SHAPE_REPRESENTATION(#153,#13235);
#232=CONTEXT_DEPENDENT_SHAPE_REPRESENTATION(#154,#13236);
#233=CONTEXT_DEPENDENT_SHAPE_REPRESENTATION(#155,#13237);
#234=CONTEXT_DEPENDENT_SHAPE_REPRESENTATION(#156,#13238);
#235=CONTEXT_DEPENDENT_SHAPE_REPRESENTATION(#157,#13239);
#236=CONTEXT_DEPENDENT_SHAPE_REPRESENTATION(#158,#13240);
#237=CONTEXT_DEPENDENT_SHAPE_REPRESENTATION(#159,#13241);
#238=CONTEXT_DEPENDENT_SHAPE_REPRESENTATION(#160,#13242);
#239=CONTEXT_DEPENDENT_SHAPE_REPRESENTATION(#161,#13243);
#240=CONTEXT_DEPENDENT_SHAPE_REPRESENTATION(#162,#13244);
#241=CONTEXT_DEPENDENT_SHAPE_REPRESENTATION(#163,#13245);
#242=CONTEXT_DEPENDENT_SHAPE_REPRESENTATION(#164,#13246);
#243=CONTEXT_DEPENDENT_SHAPE_REPRESENTATION(#165,#13247);
#244=CONTEXT_DEPENDENT_SHAPE_REPRESENTATION(#166,#13248);
#245=NEXT_ASSEMBLY_USAGE_OCCURRENCE('Block:1','Block:1','Block:1',#13316,
#13317,'Block:1');
#246=NEXT_ASSEMBLY_USAGE_OCCURRENCE('End cap +:1','End cap +:1',
'End cap +:1',#13316,#13318,'End cap +:1');
#247=NEXT_ASSEMBLY_USAGE_OCCURRENCE('End cap:1','End cap:1','End cap:1',
#13316,#13319,'End cap:1');
#248=NEXT_ASSEMBLY_USAGE_OCCURRENCE('Base:1','Base:1','Base:1',#13287,#13288,
'Base:1');
#249=NEXT_ASSEMBLY_USAGE_OCCURRENCE('Top frame:1','Top frame:1',
'Top frame:1',#13287,#13289,'Top frame:1');
#250=NEXT_ASSEMBLY_USAGE_OCCURRENCE('Foot strip:1','Foot strip:1',
'Foot strip:1',#13287,#13290,'Foot strip:1');
#251=NEXT_ASSEMBLY_USAGE_OCCURRENCE('Foot strip (1):1',
'Foot strip (1):1','Foot strip (1):1',#13287,#13291,'Foot strip (1):1');
#252=NEXT_ASSEMBLY_USAGE_OCCURRENCE('Chute floor:1','Chute floor:1',
'Chute floor:1',#13287,#13292,'Chute floor:1');
#253=NEXT_ASSEMBLY_USAGE_OCCURRENCE('Chute side:1','Chute side:1',
'Chute side:1',#13287,#13293,'Chute side:1');
#254=NEXT_ASSEMBLY_USAGE_OCCURRENCE('Chute side (1):1',
'Chute side (1):1','Chute side (1):1',#13287,#13294,'Chute side (1):1');
#255=NEXT_ASSEMBLY_USAGE_OCCURRENCE('Chute support bracket:1',
'Chute support bracket:1','Chute support bracket:1',#13287,#13295,
'Chute support bracket:1');
#256=NEXT_ASSEMBLY_USAGE_OCCURRENCE('Chute support bracket (1):1',
'Chute support bracket (1):1','Chute support bracket (1):1',#13287,#13296,
'Chute support bracket (1):1');
#257=NEXT_ASSEMBLY_USAGE_OCCURRENCE('Chute support bracket (2):1',
'Chute support bracket (2):1','Chute support bracket (2):1',#13287,#13297,
'Chute support bracket (2):1');
#258=NEXT_ASSEMBLY_USAGE_OCCURRENCE('Chute support bracket (3):1',
'Chute support bracket (3):1','Chute support bracket (3):1',#13287,#13298,
'Chute support bracket (3):1');
#259=NEXT_ASSEMBLY_USAGE_OCCURRENCE('Outlet frame:1','Outlet frame:1',
'Outlet frame:1',#13287,#13299,'Outlet frame:1');
#260=NEXT_ASSEMBLY_USAGE_OCCURRENCE('Gate wiper gasket:1',
'Gate wiper gasket:1','Gate wiper gasket:1',#13287,#13300,
'Gate wiper gasket:1');
#261=NEXT_ASSEMBLY_USAGE_OCCURRENCE('Rail backing bar:1',
'Rail backing bar:1','Rail backing bar:1',#13287,#13301,
'Rail backing bar:1');
#262=NEXT_ASSEMBLY_USAGE_OCCURRENCE('Left gate guide:1',
'Left gate guide:1','Left gate guide:1',#13287,#13302,
'Left gate guide:1');
#263=NEXT_ASSEMBLY_USAGE_OCCURRENCE('Gate guide bracket:1',
'Gate guide bracket:1','Gate guide bracket:1',#13287,#13303,
'Gate guide bracket:1');
#264=NEXT_ASSEMBLY_USAGE_OCCURRENCE('Gate guide bracket (1):1',
'Gate guide bracket (1):1','Gate guide bracket (1):1',#13287,#13304,
'Gate guide bracket (1):1');
#265=NEXT_ASSEMBLY_USAGE_OCCURRENCE('Gate end stop:1','Gate end stop:1',
'Gate end stop:1',#13287,#13305,'Gate end stop:1');
#266=NEXT_ASSEMBLY_USAGE_OCCURRENCE('Gate end stop (1):1',
'Gate end stop (1):1','Gate end stop (1):1',#13287,#13306,
'Gate end stop (1):1');
#267=NEXT_ASSEMBLY_USAGE_OCCURRENCE(
'Slotted Extrusion - 20 x 20 x 400 mm:2',
'Slotted Extrusion - 20 x 20 x 400 mm:2',
'Slotted Extrusion - 20 x 20 x 400 mm:2',#13287,#13307,
'Slotted Extrusion - 20 x 20 x 400 mm:2');
#268=NEXT_ASSEMBLY_USAGE_OCCURRENCE('Cap Screw - M5x20:2',
'Cap Screw - M5x20:2','Cap Screw - M5x20:2',#13287,#13308,
'Cap Screw - M5x20:2');
#269=NEXT_ASSEMBLY_USAGE_OCCURRENCE('Cap Screw - M5x20:3',
'Cap Screw - M5x20:3','Cap Screw - M5x20:3',#13287,#13308,
'Cap Screw - M5x20:3');
#270=NEXT_ASSEMBLY_USAGE_OCCURRENCE(
'Slotted Extrusion - 20 x 20 x 400 mm:3',
'Slotted Extrusion - 20 x 20 x 400 mm:3',
'Slotted Extrusion - 20 x 20 x 400 mm:3',#13287,#13307,
'Slotted Extrusion - 20 x 20 x 400 mm:3');
#271=NEXT_ASSEMBLY_USAGE_OCCURRENCE('Cap Screw - M5x20:4',
'Cap Screw - M5x20:4','Cap Screw - M5x20:4',#13287,#13308,
'Cap Screw - M5x20:4');
#272=NEXT_ASSEMBLY_USAGE_OCCURRENCE('Cap Screw - M5x20:5',
'Cap Screw - M5x20:5','Cap Screw - M5x20:5',#13287,#13308,
'Cap Screw - M5x20:5');
#273=NEXT_ASSEMBLY_USAGE_OCCURRENCE(
'Slotted Extrusion - 20 x 20 x 400 mm:4',
'Slotted Extrusion - 20 x 20 x 400 mm:4',
'Slotted Extrusion - 20 x 20 x 400 mm:4',#13287,#13307,
'Slotted Extrusion - 20 x 20 x 400 mm:4');
#274=NEXT_ASSEMBLY_USAGE_OCCURRENCE('Cap Screw - M5x20:6',
'Cap Screw - M5x20:6','Cap Screw - M5x20:6',#13287,#13308,
'Cap Screw - M5x20:6');
#275=NEXT_ASSEMBLY_USAGE_OCCURRENCE('Cap Screw - M5x20:7',
'Cap Screw - M5x20:7','Cap Screw - M5x20:7',#13287,#13308,
'Cap Screw - M5x20:7');
#276=NEXT_ASSEMBLY_USAGE_OCCURRENCE(
'Slotted Extrusion - 20 x 20 x 400 mm:5',
'Slotted Extrusion - 20 x 20 x 400 mm:5',
'Slotted Extrusion - 20 x 20 x 400 mm:5',#13287,#13307,
'Slotted Extrusion - 20 x 20 x 400 mm:5');
#277=NEXT_ASSEMBLY_USAGE_OCCURRENCE('Cap Screw - M5x20:8',
'Cap Screw - M5x20:8','Cap Screw - M5x20:8',#13287,#13308,
'Cap Screw - M5x20:8');
#278=NEXT_ASSEMBLY_USAGE_OCCURRENCE('Cap Screw - M5x20:9',
'Cap Screw - M5x20:9','Cap Screw - M5x20:9',#13287,#13308,
'Cap Screw - M5x20:9');
#279=NEXT_ASSEMBLY_USAGE_OCCURRENCE('Captive slot nut:2',
'Captive slot nut:2','Captive slot nut:2',#13287,#13310,
'Captive slot nut:2');
#280=NEXT_ASSEMBLY_USAGE_OCCURRENCE('Cap Screw - M5x20:10',
'Cap Screw - M5x20:10','Cap Screw - M5x20:10',#13287,#13308,
'Cap Screw - M5x20:10');
#281=NEXT_ASSEMBLY_USAGE_OCCURRENCE('Cap Screw - M4x16:2',
'Cap Screw - M4x16:2','Cap Screw - M4x16:2',#13287,#13321,
'Cap Screw - M4x16:2');
#282=NEXT_ASSEMBLY_USAGE_OCCURRENCE('Captive slot nut:3',
'Captive slot nut:3','Captive slot nut:3',#13287,#13310,
'Captive slot nut:3');
#283=NEXT_ASSEMBLY_USAGE_OCCURRENCE('Cap Screw - M5x20:11',
'Cap Screw - M5x20:11','Cap Screw - M5x20:11',#13287,#13308,
'Cap Screw - M5x20:11');
#284=NEXT_ASSEMBLY_USAGE_OCCURRENCE('Cap Screw - M4x16:3',
'Cap Screw - M4x16:3','Cap Screw - M4x16:3',#13287,#13321,
'Cap Screw - M4x16:3');
#285=NEXT_ASSEMBLY_USAGE_OCCURRENCE('Captive slot nut:4',
'Captive slot nut:4','Captive slot nut:4',#13287,#13310,
'Captive slot nut:4');
#286=NEXT_ASSEMBLY_USAGE_OCCURRENCE('Cap Screw - M5x20:12',
'Cap Screw - M5x20:12','Cap Screw - M5x20:12',#13287,#13308,
'Cap Screw - M5x20:12');
#287=NEXT_ASSEMBLY_USAGE_OCCURRENCE('Cap Screw - M4x16:4',
'Cap Screw - M4x16:4','Cap Screw - M4x16:4',#13287,#13321,
'Cap Screw - M4x16:4');
#288=NEXT_ASSEMBLY_USAGE_OCCURRENCE('Captive slot nut:5',
'Captive slot nut:5','Captive slot nut:5',#13287,#13310,
'Captive slot nut:5');
#289=NEXT_ASSEMBLY_USAGE_OCCURRENCE('Cap Screw - M5x20:13',
'Cap Screw - M5x20:13','Cap Screw - M5x20:13',#13287,#13308,
'Cap Screw - M5x20:13');
#290=NEXT_ASSEMBLY_USAGE_OCCURRENCE('Cap Screw - M4x16:5',
'Cap Screw - M4x16:5','Cap Screw - M4x16:5',#13287,#13321,
'Cap Screw - M4x16:5');
#291=NEXT_ASSEMBLY_USAGE_OCCURRENCE('Captive slot nut:6',
'Captive slot nut:6','Captive slot nut:6',#13287,#13310,
'Captive slot nut:6');
#292=NEXT_ASSEMBLY_USAGE_OCCURRENCE('Flat Washer - M5:2',
'Flat Washer - M5:2','Flat Washer - M5:2',#13287,#13311,
'Flat Washer - M5:2');
#293=NEXT_ASSEMBLY_USAGE_OCCURRENCE('M5x14 Cap Screw:2',
'M5x14 Cap Screw:2','M5x14 Cap Screw:2',#13287,#13320,
'M5x14 Cap Screw:2');
#294=NEXT_ASSEMBLY_USAGE_OCCURRENCE('Captive slot nut:7',
'Captive slot nut:7','Captive slot nut:7',#13287,#13310,
'Captive slot nut:7');
#295=NEXT_ASSEMBLY_USAGE_OCCURRENCE('Flat Washer - M5:3',
'Flat Washer - M5:3','Flat Washer - M5:3',#13287,#13311,
'Flat Washer - M5:3');
#296=NEXT_ASSEMBLY_USAGE_OCCURRENCE('M5x14 Cap Screw:3',
'M5x14 Cap Screw:3','M5x14 Cap Screw:3',#13287,#13320,
'M5x14 Cap Screw:3');
#297=NEXT_ASSEMBLY_USAGE_OCCURRENCE(
'Linear Guide Rail - 15 mm, 220 mm Long:2',
'Linear Guide Rail - 15 mm, 220 mm Long:2',
'Linear Guide Rail - 15 mm, 220 mm Long:2',#13287,#13309,
'Linear Guide Rail - 15 mm, 220 mm Long:2');
#298=NEXT_ASSEMBLY_USAGE_OCCURRENCE('Cap Screw - M4x16:6',
'Cap Screw - M4x16:6','Cap Screw - M4x16:6',#13287,#13321,
'Cap Screw - M4x16:6');
#299=NEXT_ASSEMBLY_USAGE_OCCURRENCE('Cap Screw - M4x16:7',
'Cap Screw - M4x16:7','Cap Screw - M4x16:7',#13287,#13321,
'Cap Screw - M4x16:7');
#300=NEXT_ASSEMBLY_USAGE_OCCURRENCE('Cap Screw - M4x16:8',
'Cap Screw - M4x16:8','Cap Screw - M4x16:8',#13287,#13321,
'Cap Screw - M4x16:8');
#301=NEXT_ASSEMBLY_USAGE_OCCURRENCE('Cap Screw - M4x16:9',
'Cap Screw - M4x16:9','Cap Screw - M4x16:9',#13287,#13321,
'Cap Screw - M4x16:9');
#302=NEXT_ASSEMBLY_USAGE_OCCURRENCE('Captive slot nut:8',
'Captive slot nut:8','Captive slot nut:8',#13287,#13310,
'Captive slot nut:8');
#303=NEXT_ASSEMBLY_USAGE_OCCURRENCE('Flat Washer - M5:4',
'Flat Washer - M5:4','Flat Washer - M5:4',#13287,#13311,
'Flat Washer - M5:4');
#304=NEXT_ASSEMBLY_USAGE_OCCURRENCE('M5x14 Cap Screw:8',
'M5x14 Cap Screw:8','M5x14 Cap Screw:8',#13287,#13320,
'M5x14 Cap Screw:8');
#305=NEXT_ASSEMBLY_USAGE_OCCURRENCE('Cap Screw - M4x16:10',
'Cap Screw - M4x16:10','Cap Screw - M4x16:10',#13287,#13321,
'Cap Screw - M4x16:10');
#306=NEXT_ASSEMBLY_USAGE_OCCURRENCE('Captive slot nut:9',
'Captive slot nut:9','Captive slot nut:9',#13287,#13310,
'Captive slot nut:9');
#307=NEXT_ASSEMBLY_USAGE_OCCURRENCE('Flat Washer - M5:5',
'Flat Washer - M5:5','Flat Washer - M5:5',#13287,#13311,
'Flat Washer - M5:5');
#308=NEXT_ASSEMBLY_USAGE_OCCURRENCE('M5x14 Cap Screw:9',
'M5x14 Cap Screw:9','M5x14 Cap Screw:9',#13287,#13320,
'M5x14 Cap Screw:9');
#309=NEXT_ASSEMBLY_USAGE_OCCURRENCE('Cap Screw - M4x16:11',
'Cap Screw - M4x16:11','Cap Screw - M4x16:11',#13287,#13321,
'Cap Screw - M4x16:11');
#310=NEXT_ASSEMBLY_USAGE_OCCURRENCE('M5x30 frame screw:2',
'M5x30 frame screw:2','M5x30 frame screw:2',#13287,#13312,
'M5x30 frame screw:2');
#311=NEXT_ASSEMBLY_USAGE_OCCURRENCE('M5x30 frame screw:3',
'M5x30 frame screw:3','M5x30 frame screw:3',#13287,#13312,
'M5x30 frame screw:3');
#312=NEXT_ASSEMBLY_USAGE_OCCURRENCE('Gate panel:1','Gate panel:1',
'Gate panel:1',#13313,#13314,'Gate panel:1');
#313=NEXT_ASSEMBLY_USAGE_OCCURRENCE('Gate grip:1','Gate grip:1',
'Gate grip:1',#13313,#13315,'Gate grip:1');
#314=NEXT_ASSEMBLY_USAGE_OCCURRENCE(
'Flanged Linear Guide Carriage - 15 mm:2',
'Flanged Linear Guide Carriage - 15 mm:2',
'Flanged Linear Guide Carriage - 15 mm:2',#13313,#13316,
'Flanged Linear Guide Carriage - 15 mm:2');
#315=NEXT_ASSEMBLY_USAGE_OCCURRENCE('M5x14 Cap Screw:4',
'M5x14 Cap Screw:4','M5x14 Cap Screw:4',#13313,#13320,
'M5x14 Cap Screw:4');
#316=NEXT_ASSEMBLY_USAGE_OCCURRENCE('M5x14 Cap Screw:5',
'M5x14 Cap Screw:5','M5x14 Cap Screw:5',#13313,#13320,
'M5x14 Cap Screw:5');
#317=NEXT_ASSEMBLY_USAGE_OCCURRENCE('M5x14 Cap Screw:6',
'M5x14 Cap Screw:6','M5x14 Cap Screw:6',#13313,#13320,
'M5x14 Cap Screw:6');
#318=NEXT_ASSEMBLY_USAGE_OCCURRENCE('M5x14 Cap Screw:7',
'M5x14 Cap Screw:7','M5x14 Cap Screw:7',#13313,#13320,
'M5x14 Cap Screw:7');
#319=NEXT_ASSEMBLY_USAGE_OCCURRENCE('Cap Screw - M4x16:12',
'Cap Screw - M4x16:12','Cap Screw - M4x16:12',#13313,#13321,
'Cap Screw - M4x16:12');
#320=NEXT_ASSEMBLY_USAGE_OCCURRENCE('Cap Screw - M4x16:13',
'Cap Screw - M4x16:13','Cap Screw - M4x16:13',#13313,#13321,
'Cap Screw - M4x16:13');
#321=NEXT_ASSEMBLY_USAGE_OCCURRENCE('Chute and extrusion frame:1',
'Chute and extrusion frame:1','Chute and extrusion frame:1',#13286,#13287,
'Chute and extrusion frame:1');
#322=NEXT_ASSEMBLY_USAGE_OCCURRENCE('Gate and handle:1',
'Gate and handle:1','Gate and handle:1',#13286,#13313,
'Gate and handle:1');
#323=ELLIPSE('',#8401,0.299389011154384,0.2117);
#324=ELLIPSE('',#8405,0.299389011154384,0.2117);
#325=ELLIPSE('',#8491,0.707106781186548,0.5);
#326=ELLIPSE('',#8501,0.707106781186548,0.5);
#327=ORIENTED_CLOSED_SHELL('',*,#7618,.F.);
#328=ORIENTED_CLOSED_SHELL('',*,#7622,.F.);
#329=ORIENTED_CLOSED_SHELL('',*,#7629,.F.);
#330=ORIENTED_CLOSED_SHELL('',*,#7632,.F.);
#331=CONICAL_SURFACE('',#8324,0.4,0.785398163397448);
#332=CONICAL_SURFACE('',#8328,0.41,0.785398163397448);
#333=CONICAL_SURFACE('',#8332,0.26,0.463647609000806);
#334=CONICAL_SURFACE('',#8336,0.225,0.785398163397448);
#335=CONICAL_SURFACE('',#8412,0.275,0.785398163397449);
#336=CONICAL_SURFACE('',#8439,0.4,0.785398163397448);
#337=CONICAL_SURFACE('',#8443,0.41,0.785398163397448);
#338=CONICAL_SURFACE('',#8447,0.26,0.463647609000806);
#339=CONICAL_SURFACE('',#8586,0.4,0.785398163397448);
#340=CONICAL_SURFACE('',#8590,0.41,0.785398163397448);
#341=CONICAL_SURFACE('',#8594,0.26,0.463647609000806);
#342=CONICAL_SURFACE('',#8600,0.325,0.785398163397448);
#343=CONICAL_SURFACE('',#8604,0.335,0.785398163397448);
#344=CONICAL_SURFACE('',#8608,0.21,0.463647609000806);
#345=CONICAL_SURFACE('',#8612,0.18,0.785398163397448);
#346=BREP_WITH_VOIDS('Body1',#7617,(#327));
#347=BREP_WITH_VOIDS('Body1',#7623,(#328));
#348=BREP_WITH_VOIDS('Body1',#7630,(#329));
#349=BREP_WITH_VOIDS('Body1',#7631,(#330));
#350=SHAPE_REPRESENTATION_RELATIONSHIP('SRR','None',#13251,#382);
#351=SHAPE_REPRESENTATION_RELATIONSHIP('SRR','None',#13252,#383);
#352=SHAPE_REPRESENTATION_RELATIONSHIP('SRR','None',#13253,#384);
#353=SHAPE_REPRESENTATION_RELATIONSHIP('SRR','None',#13254,#385);
#354=SHAPE_REPRESENTATION_RELATIONSHIP('SRR','None',#13255,#386);
#355=SHAPE_REPRESENTATION_RELATIONSHIP('SRR','None',#13256,#387);
#356=SHAPE_REPRESENTATION_RELATIONSHIP('SRR','None',#13257,#388);
#357=SHAPE_REPRESENTATION_RELATIONSHIP('SRR','None',#13258,#389);
#358=SHAPE_REPRESENTATION_RELATIONSHIP('SRR','None',#13259,#390);
#359=SHAPE_REPRESENTATION_RELATIONSHIP('SRR','None',#13260,#391);
#360=SHAPE_REPRESENTATION_RELATIONSHIP('SRR','None',#13261,#392);
#361=SHAPE_REPRESENTATION_RELATIONSHIP('SRR','None',#13262,#393);
#362=SHAPE_REPRESENTATION_RELATIONSHIP('SRR','None',#13263,#394);
#363=SHAPE_REPRESENTATION_RELATIONSHIP('SRR','None',#13264,#395);
#364=SHAPE_REPRESENTATION_RELATIONSHIP('SRR','None',#13265,#396);
#365=SHAPE_REPRESENTATION_RELATIONSHIP('SRR','None',#13266,#397);
#366=SHAPE_REPRESENTATION_RELATIONSHIP('SRR','None',#13267,#398);
#367=SHAPE_REPRESENTATION_RELATIONSHIP('SRR','None',#13268,#399);
#368=SHAPE_REPRESENTATION_RELATIONSHIP('SRR','None',#13269,#400);
#369=SHAPE_REPRESENTATION_RELATIONSHIP('SRR','None',#13270,#401);
#370=SHAPE_REPRESENTATION_RELATIONSHIP('SRR','None',#13271,#402);
#371=SHAPE_REPRESENTATION_RELATIONSHIP('SRR','None',#13272,#403);
#372=SHAPE_REPRESENTATION_RELATIONSHIP('SRR','None',#13273,#404);
#373=SHAPE_REPRESENTATION_RELATIONSHIP('SRR','None',#13274,#405);
#374=SHAPE_REPRESENTATION_RELATIONSHIP('SRR','None',#13275,#406);
#375=SHAPE_REPRESENTATION_RELATIONSHIP('SRR','None',#13277,#407);
#376=SHAPE_REPRESENTATION_RELATIONSHIP('SRR','None',#13278,#408);
#377=SHAPE_REPRESENTATION_RELATIONSHIP('SRR','None',#13280,#409);
#378=SHAPE_REPRESENTATION_RELATIONSHIP('SRR','None',#13281,#410);
#379=SHAPE_REPRESENTATION_RELATIONSHIP('SRR','None',#13282,#411);
#380=SHAPE_REPRESENTATION_RELATIONSHIP('SRR','None',#13283,#412);
#381=SHAPE_REPRESENTATION_RELATIONSHIP('SRR','None',#13284,#413);
#382=ADVANCED_BREP_SHAPE_REPRESENTATION('',(#446),#13060);
#383=ADVANCED_BREP_SHAPE_REPRESENTATION('',(#447),#13061);
#384=ADVANCED_BREP_SHAPE_REPRESENTATION('',(#448),#13062);
#385=ADVANCED_BREP_SHAPE_REPRESENTATION('',(#449),#13063);
#386=ADVANCED_BREP_SHAPE_REPRESENTATION('',(#450),#13064);
#387=ADVANCED_BREP_SHAPE_REPRESENTATION('',(#451),#13065);
#388=ADVANCED_BREP_SHAPE_REPRESENTATION('',(#452),#13066);
#389=ADVANCED_BREP_SHAPE_REPRESENTATION('',(#453),#13067);
#390=ADVANCED_BREP_SHAPE_REPRESENTATION('',(#454),#13068);
#391=ADVANCED_BREP_SHAPE_REPRESENTATION('',(#455),#13069);
#392=ADVANCED_BREP_SHAPE_REPRESENTATION('',(#456),#13070);
#393=ADVANCED_BREP_SHAPE_REPRESENTATION('',(#457),#13071);
#394=ADVANCED_BREP_SHAPE_REPRESENTATION('',(#458),#13072);
#395=ADVANCED_BREP_SHAPE_REPRESENTATION('',(#459),#13073);
#396=ADVANCED_BREP_SHAPE_REPRESENTATION('',(#460),#13074);
#397=ADVANCED_BREP_SHAPE_REPRESENTATION('',(#461),#13075);
#398=ADVANCED_BREP_SHAPE_REPRESENTATION('',(#462),#13076);
#399=ADVANCED_BREP_SHAPE_REPRESENTATION('',(#463),#13077);
#400=ADVANCED_BREP_SHAPE_REPRESENTATION('',(#464),#13078);
#401=ADVANCED_BREP_SHAPE_REPRESENTATION('',(#465),#13079);
#402=ADVANCED_BREP_SHAPE_REPRESENTATION('',(#346),#13080);
#403=ADVANCED_BREP_SHAPE_REPRESENTATION('',(#466),#13081);
#404=ADVANCED_BREP_SHAPE_REPRESENTATION('',(#467),#13082);
#405=ADVANCED_BREP_SHAPE_REPRESENTATION('',(#468),#13083);
#406=ADVANCED_BREP_SHAPE_REPRESENTATION('',(#347),#13084);
#407=ADVANCED_BREP_SHAPE_REPRESENTATION('',(#469),#13086);
#408=ADVANCED_BREP_SHAPE_REPRESENTATION('',(#470),#13087);
#409=ADVANCED_BREP_SHAPE_REPRESENTATION('',(#471),#13089);
#410=ADVANCED_BREP_SHAPE_REPRESENTATION('',(#472),#13090);
#411=ADVANCED_BREP_SHAPE_REPRESENTATION('',(#473),#13091);
#412=ADVANCED_BREP_SHAPE_REPRESENTATION('',(#348),#13092);
#413=ADVANCED_BREP_SHAPE_REPRESENTATION('',(#349),#13093);
#414=STYLED_ITEM('',(#13474),#446);
#415=STYLED_ITEM('',(#13474),#447);
#416=STYLED_ITEM('',(#13481),#448);
#417=STYLED_ITEM('',(#13481),#449);
#418=STYLED_ITEM('',(#13481),#450);
#419=STYLED_ITEM('',(#13509),#451);
#420=STYLED_ITEM('',(#13509),#452);
#421=STYLED_ITEM('',(#13474),#453);
#422=STYLED_ITEM('',(#13474),#454);
#423=STYLED_ITEM('',(#13474),#455);
#424=STYLED_ITEM('',(#13474),#456);
#425=STYLED_ITEM('',(#13474),#457);
#426=STYLED_ITEM('',(#13481),#458);
#427=STYLED_ITEM('',(#13481),#459);
#428=STYLED_ITEM('',(#13509),#460);
#429=STYLED_ITEM('',(#13474),#461);
#430=STYLED_ITEM('',(#13474),#462);
#431=STYLED_ITEM('',(#13481),#463);
#432=STYLED_ITEM('',(#13481),#464);
#433=STYLED_ITEM('',(#13481),#465);
#434=STYLED_ITEM('',(#13502),#346);
#435=STYLED_ITEM('',(#13488),#466);
#436=STYLED_ITEM('',(#13502),#467);
#437=STYLED_ITEM('',(#13502),#468);
#438=STYLED_ITEM('',(#13502),#347);
#439=STYLED_ITEM('',(#13488),#469);
#440=STYLED_ITEM('',(#13502),#470);
#441=STYLED_ITEM('',(#13474),#471);
#442=STYLED_ITEM('',(#13488),#472);
#443=STYLED_ITEM('',(#13509),#473);
#444=STYLED_ITEM('',(#13502),#348);
#445=STYLED_ITEM('',(#13502),#349);
#446=MANIFOLD_SOLID_BREP('Body1',#7597);
#447=MANIFOLD_SOLID_BREP('Body1',#7598);
#448=MANIFOLD_SOLID_BREP('Body1',#7599);
#449=MANIFOLD_SOLID_BREP('Body1',#7600);
#450=MANIFOLD_SOLID_BREP('Body1',#7601);
#451=MANIFOLD_SOLID_BREP('Body1',#7602);
#452=MANIFOLD_SOLID_BREP('Body1',#7603);
#453=MANIFOLD_SOLID_BREP('Body1',#7604);
#454=MANIFOLD_SOLID_BREP('Body1',#7605);
#455=MANIFOLD_SOLID_BREP('Body1',#7606);
#456=MANIFOLD_SOLID_BREP('Body1',#7607);
#457=MANIFOLD_SOLID_BREP('Body1',#7608);
#458=MANIFOLD_SOLID_BREP('Body1',#7609);
#459=MANIFOLD_SOLID_BREP('Body1',#7610);
#460=MANIFOLD_SOLID_BREP('Body1',#7611);
#461=MANIFOLD_SOLID_BREP('Body1',#7612);
#462=MANIFOLD_SOLID_BREP('Body1',#7613);
#463=MANIFOLD_SOLID_BREP('Body1',#7614);
#464=MANIFOLD_SOLID_BREP('Body1',#7615);
#465=MANIFOLD_SOLID_BREP('Body1',#7616);
#466=MANIFOLD_SOLID_BREP('Body1',#7619);
#467=MANIFOLD_SOLID_BREP('Body1',#7620);
#468=MANIFOLD_SOLID_BREP('Body1',#7621);
#469=MANIFOLD_SOLID_BREP('Body1',#7624);
#470=MANIFOLD_SOLID_BREP('Body1',#7625);
#471=MANIFOLD_SOLID_BREP('Body1',#7626);
#472=MANIFOLD_SOLID_BREP('Body1',#7627);
#473=MANIFOLD_SOLID_BREP('Body1',#7628);
#474=FACE_BOUND('',#1338,.T.);
#475=FACE_BOUND('',#1339,.T.);
#476=FACE_BOUND('',#1340,.T.);
#477=FACE_BOUND('',#1341,.T.);
#478=FACE_BOUND('',#1343,.T.);
#479=FACE_BOUND('',#1344,.T.);
#480=FACE_BOUND('',#1345,.T.);
#481=FACE_BOUND('',#1346,.T.);
#482=FACE_BOUND('',#1360,.T.);
#483=FACE_BOUND('',#1361,.T.);
#484=FACE_BOUND('',#1362,.T.);
#485=FACE_BOUND('',#1363,.T.);
#486=FACE_BOUND('',#1364,.T.);
#487=FACE_BOUND('',#1366,.T.);
#488=FACE_BOUND('',#1367,.T.);
#489=FACE_BOUND('',#1368,.T.);
#490=FACE_BOUND('',#1369,.T.);
#491=FACE_BOUND('',#1370,.T.);
#492=FACE_BOUND('',#1396,.T.);
#493=FACE_BOUND('',#1397,.T.);
#494=FACE_BOUND('',#1399,.T.);
#495=FACE_BOUND('',#1400,.T.);
#496=FACE_BOUND('',#1408,.T.);
#497=FACE_BOUND('',#1409,.T.);
#498=FACE_BOUND('',#1411,.T.);
#499=FACE_BOUND('',#1412,.T.);
#500=FACE_BOUND('',#1417,.T.);
#501=FACE_BOUND('',#1420,.T.);
#502=FACE_BOUND('',#1421,.T.);
#503=FACE_BOUND('',#1424,.T.);
#504=FACE_BOUND('',#1432,.T.);
#505=FACE_BOUND('',#1435,.T.);
#506=FACE_BOUND('',#1438,.T.);
#507=FACE_BOUND('',#1439,.T.);
#508=FACE_BOUND('',#1447,.T.);
#509=FACE_BOUND('',#1450,.T.);
#510=FACE_BOUND('',#1451,.T.);
#511=FACE_BOUND('',#1454,.T.);
#512=FACE_BOUND('',#1462,.T.);
#513=FACE_BOUND('',#1465,.T.);
#514=FACE_BOUND('',#1468,.T.);
#515=FACE_BOUND('',#1469,.T.);
#516=FACE_BOUND('',#1482,.T.);
#517=FACE_BOUND('',#1484,.T.);
#518=FACE_BOUND('',#1494,.T.);
#519=FACE_BOUND('',#1496,.T.);
#520=FACE_BOUND('',#1507,.T.);
#521=FACE_BOUND('',#1508,.T.);
#522=FACE_BOUND('',#1509,.T.);
#523=FACE_BOUND('',#1510,.T.);
#524=FACE_BOUND('',#1511,.T.);
#525=FACE_BOUND('',#1512,.T.);
#526=FACE_BOUND('',#1513,.T.);
#527=FACE_BOUND('',#1514,.T.);
#528=FACE_BOUND('',#1517,.T.);
#529=FACE_BOUND('',#1518,.T.);
#530=FACE_BOUND('',#1519,.T.);
#531=FACE_BOUND('',#1520,.T.);
#532=FACE_BOUND('',#1521,.T.);
#533=FACE_BOUND('',#1522,.T.);
#534=FACE_BOUND('',#1523,.T.);
#535=FACE_BOUND('',#1524,.T.);
#536=FACE_BOUND('',#1533,.T.);
#537=FACE_BOUND('',#1534,.T.);
#538=FACE_BOUND('',#1537,.T.);
#539=FACE_BOUND('',#1538,.T.);
#540=FACE_BOUND('',#1546,.T.);
#541=FACE_BOUND('',#1551,.T.);
#542=FACE_BOUND('',#1554,.T.);
#543=FACE_BOUND('',#1561,.T.);
#544=FACE_BOUND('',#1566,.T.);
#545=FACE_BOUND('',#1569,.T.);
#546=FACE_BOUND('',#1574,.T.);
#547=FACE_BOUND('',#1577,.T.);
#548=FACE_BOUND('',#1583,.T.);
#549=FACE_BOUND('',#1586,.T.);
#550=FACE_BOUND('',#1635,.T.);
#551=FACE_BOUND('',#1637,.T.);
#552=FACE_BOUND('',#1643,.T.);
#553=FACE_BOUND('',#1658,.T.);
#554=FACE_BOUND('',#1661,.T.);
#555=FACE_BOUND('',#1664,.T.);
#556=FACE_BOUND('',#1667,.T.);
#557=FACE_BOUND('',#1677,.T.);
#558=FACE_BOUND('',#1678,.T.);
#559=FACE_BOUND('',#1679,.T.);
#560=FACE_BOUND('',#1680,.T.);
#561=FACE_BOUND('',#1687,.T.);
#562=FACE_BOUND('',#1688,.T.);
#563=FACE_BOUND('',#1689,.T.);
#564=FACE_BOUND('',#1690,.T.);
#565=FACE_BOUND('',#1697,.T.);
#566=FACE_BOUND('',#1712,.T.);
#567=FACE_BOUND('',#1715,.T.);
#568=FACE_BOUND('',#1725,.T.);
#569=FACE_BOUND('',#1733,.T.);
#570=FACE_BOUND('',#1746,.T.);
#571=FACE_BOUND('',#1747,.T.);
#572=FACE_BOUND('',#1748,.T.);
#573=FACE_BOUND('',#1749,.T.);
#574=FACE_BOUND('',#1750,.T.);
#575=FACE_BOUND('',#1751,.T.);
#576=FACE_BOUND('',#1758,.T.);
#577=FACE_BOUND('',#1759,.T.);
#578=FACE_BOUND('',#1760,.T.);
#579=FACE_BOUND('',#1761,.T.);
#580=FACE_BOUND('',#1762,.T.);
#581=FACE_BOUND('',#1763,.T.);
#582=FACE_BOUND('',#1770,.T.);
#583=FACE_BOUND('',#1775,.T.);
#584=FACE_BOUND('',#1793,.T.);
#585=FACE_BOUND('',#1794,.T.);
#586=FACE_BOUND('',#1795,.T.);
#587=FACE_BOUND('',#1796,.T.);
#588=FACE_BOUND('',#1839,.T.);
#589=FACE_BOUND('',#1847,.T.);
#590=PLANE('',#8001);
#591=PLANE('',#8002);
#592=PLANE('',#8003);
#593=PLANE('',#8004);
#594=PLANE('',#8005);
#595=PLANE('',#8006);
#596=PLANE('',#8020);
#597=PLANE('',#8021);
#598=PLANE('',#8022);
#599=PLANE('',#8023);
#600=PLANE('',#8024);
#601=PLANE('',#8025);
#602=PLANE('',#8026);
#603=PLANE('',#8027);
#604=PLANE('',#8028);
#605=PLANE('',#8029);
#606=PLANE('',#8031);
#607=PLANE('',#8032);
#608=PLANE('',#8033);
#609=PLANE('',#8034);
#610=PLANE('',#8035);
#611=PLANE('',#8036);
#612=PLANE('',#8038);
#613=PLANE('',#8039);
#614=PLANE('',#8040);
#615=PLANE('',#8041);
#616=PLANE('',#8042);
#617=PLANE('',#8043);
#618=PLANE('',#8045);
#619=PLANE('',#8046);
#620=PLANE('',#8047);
#621=PLANE('',#8048);
#622=PLANE('',#8049);
#623=PLANE('',#8050);
#624=PLANE('',#8058);
#625=PLANE('',#8059);
#626=PLANE('',#8060);
#627=PLANE('',#8061);
#628=PLANE('',#8062);
#629=PLANE('',#8063);
#630=PLANE('',#8071);
#631=PLANE('',#8072);
#632=PLANE('',#8073);
#633=PLANE('',#8074);
#634=PLANE('',#8075);
#635=PLANE('',#8076);
#636=PLANE('',#8081);
#637=PLANE('',#8085);
#638=PLANE('',#8089);
#639=PLANE('',#8090);
#640=PLANE('',#8091);
#641=PLANE('',#8092);
#642=PLANE('',#8093);
#643=PLANE('',#8094);
#644=PLANE('',#8099);
#645=PLANE('',#8103);
#646=PLANE('',#8107);
#647=PLANE('',#8108);
#648=PLANE('',#8109);
#649=PLANE('',#8110);
#650=PLANE('',#8111);
#651=PLANE('',#8112);
#652=PLANE('',#8117);
#653=PLANE('',#8121);
#654=PLANE('',#8125);
#655=PLANE('',#8126);
#656=PLANE('',#8127);
#657=PLANE('',#8128);
#658=PLANE('',#8129);
#659=PLANE('',#8130);
#660=PLANE('',#8135);
#661=PLANE('',#8139);
#662=PLANE('',#8143);
#663=PLANE('',#8144);
#664=PLANE('',#8145);
#665=PLANE('',#8146);
#666=PLANE('',#8147);
#667=PLANE('',#8148);
#668=PLANE('',#8150);
#669=PLANE('',#8151);
#670=PLANE('',#8152);
#671=PLANE('',#8153);
#672=PLANE('',#8154);
#673=PLANE('',#8155);
#674=PLANE('',#8156);
#675=PLANE('',#8157);
#676=PLANE('',#8158);
#677=PLANE('',#8159);
#678=PLANE('',#8161);
#679=PLANE('',#8162);
#680=PLANE('',#8163);
#681=PLANE('',#8164);
#682=PLANE('',#8165);
#683=PLANE('',#8166);
#684=PLANE('',#8167);
#685=PLANE('',#8168);
#686=PLANE('',#8169);
#687=PLANE('',#8170);
#688=PLANE('',#8196);
#689=PLANE('',#8197);
#690=PLANE('',#8198);
#691=PLANE('',#8199);
#692=PLANE('',#8200);
#693=PLANE('',#8201);
#694=PLANE('',#8209);
#695=PLANE('',#8210);
#696=PLANE('',#8211);
#697=PLANE('',#8212);
#698=PLANE('',#8213);
#699=PLANE('',#8214);
#700=PLANE('',#8215);
#701=PLANE('',#8216);
#702=PLANE('',#8221);
#703=PLANE('',#8225);
#704=PLANE('',#8226);
#705=PLANE('',#8227);
#706=PLANE('',#8228);
#707=PLANE('',#8229);
#708=PLANE('',#8230);
#709=PLANE('',#8231);
#710=PLANE('',#8232);
#711=PLANE('',#8233);
#712=PLANE('',#8238);
#713=PLANE('',#8242);
#714=PLANE('',#8243);
#715=PLANE('',#8244);
#716=PLANE('',#8245);
#717=PLANE('',#8246);
#718=PLANE('',#8247);
#719=PLANE('',#8248);
#720=PLANE('',#8249);
#721=PLANE('',#8250);
#722=PLANE('',#8255);
#723=PLANE('',#8256);
#724=PLANE('',#8257);
#725=PLANE('',#8258);
#726=PLANE('',#8259);
#727=PLANE('',#8260);
#728=PLANE('',#8265);
#729=PLANE('',#8266);
#730=PLANE('',#8267);
#731=PLANE('',#8268);
#732=PLANE('',#8269);
#733=PLANE('',#8270);
#734=PLANE('',#8272);
#735=PLANE('',#8273);
#736=PLANE('',#8274);
#737=PLANE('',#8275);
#738=PLANE('',#8276);
#739=PLANE('',#8277);
#740=PLANE('',#8278);
#741=PLANE('',#8279);
#742=PLANE('',#8280);
#743=PLANE('',#8281);
#744=PLANE('',#8282);
#745=PLANE('',#8283);
#746=PLANE('',#8284);
#747=PLANE('',#8285);
#748=PLANE('',#8286);
#749=PLANE('',#8287);
#750=PLANE('',#8288);
#751=PLANE('',#8289);
#752=PLANE('',#8290);
#753=PLANE('',#8291);
#754=PLANE('',#8292);
#755=PLANE('',#8293);
#756=PLANE('',#8294);
#757=PLANE('',#8295);
#758=PLANE('',#8296);
#759=PLANE('',#8297);
#760=PLANE('',#8298);
#761=PLANE('',#8299);
#762=PLANE('',#8300);
#763=PLANE('',#8301);
#764=PLANE('',#8302);
#765=PLANE('',#8303);
#766=PLANE('',#8304);
#767=PLANE('',#8305);
#768=PLANE('',#8306);
#769=PLANE('',#8307);
#770=PLANE('',#8311);
#771=PLANE('',#8312);
#772=PLANE('',#8313);
#773=PLANE('',#8314);
#774=PLANE('',#8315);
#775=PLANE('',#8316);
#776=PLANE('',#8317);
#777=PLANE('',#8318);
#778=PLANE('',#8319);
#779=PLANE('',#8320);
#780=PLANE('',#8322);
#781=PLANE('',#8330);
#782=PLANE('',#8338);
#783=PLANE('',#8339);
#784=PLANE('',#8340);
#785=PLANE('',#8341);
#786=PLANE('',#8342);
#787=PLANE('',#8343);
#788=PLANE('',#8344);
#789=PLANE('',#8345);
#790=PLANE('',#8346);
#791=PLANE('',#8351);
#792=PLANE('',#8356);
#793=PLANE('',#8361);
#794=PLANE('',#8366);
#795=PLANE('',#8376);
#796=PLANE('',#8377);
#797=PLANE('',#8378);
#798=PLANE('',#8379);
#799=PLANE('',#8380);
#800=PLANE('',#8381);
#801=PLANE('',#8382);
#802=PLANE('',#8383);
#803=PLANE('',#8384);
#804=PLANE('',#8385);
#805=PLANE('',#8386);
#806=PLANE('',#8387);
#807=PLANE('',#8388);
#808=PLANE('',#8389);
#809=PLANE('',#8391);
#810=PLANE('',#8392);
#811=PLANE('',#8393);
#812=PLANE('',#8395);
#813=PLANE('',#8396);
#814=PLANE('',#8397);
#815=PLANE('',#8398);
#816=PLANE('',#8399);
#817=PLANE('',#8400);
#818=PLANE('',#8407);
#819=PLANE('',#8408);
#820=PLANE('',#8409);
#821=PLANE('',#8410);
#822=PLANE('',#8417);
#823=PLANE('',#8421);
#824=PLANE('',#8423);
#825=PLANE('',#8424);
#826=PLANE('',#8425);
#827=PLANE('',#8426);
#828=PLANE('',#8427);
#829=PLANE('',#8428);
#830=PLANE('',#8429);
#831=PLANE('',#8430);
#832=PLANE('',#8431);
#833=PLANE('',#8436);
#834=PLANE('',#8437);
#835=PLANE('',#8445);
#836=PLANE('',#8470);
#837=PLANE('',#8471);
#838=PLANE('',#8472);
#839=PLANE('',#8473);
#840=PLANE('',#8474);
#841=PLANE('',#8475);
#842=PLANE('',#8476);
#843=PLANE('',#8477);
#844=PLANE('',#8478);
#845=PLANE('',#8479);
#846=PLANE('',#8484);
#847=PLANE('',#8488);
#848=PLANE('',#8493);
#849=PLANE('',#8494);
#850=PLANE('',#8495);
#851=PLANE('',#8502);
#852=PLANE('',#8503);
#853=PLANE('',#8504);
#854=PLANE('',#8510);
#855=PLANE('',#8516);
#856=PLANE('',#8522);
#857=PLANE('',#8528);
#858=PLANE('',#8534);
#859=PLANE('',#8535);
#860=PLANE('',#8536);
#861=PLANE('',#8537);
#862=PLANE('',#8538);
#863=PLANE('',#8539);
#864=PLANE('',#8540);
#865=PLANE('',#8541);
#866=PLANE('',#8542);
#867=PLANE('',#8543);
#868=PLANE('',#8544);
#869=PLANE('',#8545);
#870=PLANE('',#8546);
#871=PLANE('',#8547);
#872=PLANE('',#8549);
#873=PLANE('',#8550);
#874=PLANE('',#8551);
#875=PLANE('',#8552);
#876=PLANE('',#8553);
#877=PLANE('',#8554);
#878=PLANE('',#8555);
#879=PLANE('',#8556);
#880=PLANE('',#8557);
#881=PLANE('',#8558);
#882=PLANE('',#8560);
#883=PLANE('',#8561);
#884=PLANE('',#8562);
#885=PLANE('',#8563);
#886=PLANE('',#8564);
#887=PLANE('',#8565);
#888=PLANE('',#8566);
#889=PLANE('',#8567);
#890=PLANE('',#8568);
#891=PLANE('',#8569);
#892=PLANE('',#8574);
#893=PLANE('',#8575);
#894=PLANE('',#8576);
#895=PLANE('',#8577);
#896=PLANE('',#8578);
#897=PLANE('',#8579);
#898=PLANE('',#8580);
#899=PLANE('',#8581);
#900=PLANE('',#8582);
#901=PLANE('',#8584);
#902=PLANE('',#8592);
#903=PLANE('',#8598);
#904=PLANE('',#8606);
#905=PLANE('',#8614);
#906=PLANE('',#8615);
#907=PLANE('',#8616);
#908=PLANE('',#8617);
#909=PLANE('',#8618);
#910=PLANE('',#8619);
#911=PLANE('',#8620);
#912=PLANE('',#8621);
#913=PLANE('',#8622);
#914=FACE_OUTER_BOUND('',#1329,.T.);
#915=FACE_OUTER_BOUND('',#1330,.T.);
#916=FACE_OUTER_BOUND('',#1331,.T.);
#917=FACE_OUTER_BOUND('',#1332,.T.);
#918=FACE_OUTER_BOUND('',#1333,.T.);
#919=FACE_OUTER_BOUND('',#1334,.T.);
#920=FACE_OUTER_BOUND('',#1335,.T.);
#921=FACE_OUTER_BOUND('',#1336,.T.);
#922=FACE_OUTER_BOUND('',#1337,.T.);
#923=FACE_OUTER_BOUND('',#1342,.T.);
#924=FACE_OUTER_BOUND('',#1347,.T.);
#925=FACE_OUTER_BOUND('',#1348,.T.);
#926=FACE_OUTER_BOUND('',#1349,.T.);
#927=FACE_OUTER_BOUND('',#1350,.T.);
#928=FACE_OUTER_BOUND('',#1351,.T.);
#929=FACE_OUTER_BOUND('',#1352,.T.);
#930=FACE_OUTER_BOUND('',#1353,.T.);
#931=FACE_OUTER_BOUND('',#1354,.T.);
#932=FACE_OUTER_BOUND('',#1355,.T.);
#933=FACE_OUTER_BOUND('',#1356,.T.);
#934=FACE_OUTER_BOUND('',#1357,.T.);
#935=FACE_OUTER_BOUND('',#1358,.T.);
#936=FACE_OUTER_BOUND('',#1359,.T.);
#937=FACE_OUTER_BOUND('',#1365,.T.);
#938=FACE_OUTER_BOUND('',#1371,.T.);
#939=FACE_OUTER_BOUND('',#1372,.T.);
#940=FACE_OUTER_BOUND('',#1373,.T.);
#941=FACE_OUTER_BOUND('',#1374,.T.);
#942=FACE_OUTER_BOUND('',#1375,.T.);
#943=FACE_OUTER_BOUND('',#1376,.T.);
#944=FACE_OUTER_BOUND('',#1377,.T.);
#945=FACE_OUTER_BOUND('',#1378,.T.);
#946=FACE_OUTER_BOUND('',#1379,.T.);
#947=FACE_OUTER_BOUND('',#1380,.T.);
#948=FACE_OUTER_BOUND('',#1381,.T.);
#949=FACE_OUTER_BOUND('',#1382,.T.);
#950=FACE_OUTER_BOUND('',#1383,.T.);
#951=FACE_OUTER_BOUND('',#1384,.T.);
#952=FACE_OUTER_BOUND('',#1385,.T.);
#953=FACE_OUTER_BOUND('',#1386,.T.);
#954=FACE_OUTER_BOUND('',#1387,.T.);
#955=FACE_OUTER_BOUND('',#1388,.T.);
#956=FACE_OUTER_BOUND('',#1389,.T.);
#957=FACE_OUTER_BOUND('',#1390,.T.);
#958=FACE_OUTER_BOUND('',#1391,.T.);
#959=FACE_OUTER_BOUND('',#1392,.T.);
#960=FACE_OUTER_BOUND('',#1393,.T.);
#961=FACE_OUTER_BOUND('',#1394,.T.);
#962=FACE_OUTER_BOUND('',#1395,.T.);
#963=FACE_OUTER_BOUND('',#1398,.T.);
#964=FACE_OUTER_BOUND('',#1401,.T.);
#965=FACE_OUTER_BOUND('',#1402,.T.);
#966=FACE_OUTER_BOUND('',#1403,.T.);
#967=FACE_OUTER_BOUND('',#1404,.T.);
#968=FACE_OUTER_BOUND('',#1405,.T.);
#969=FACE_OUTER_BOUND('',#1406,.T.);
#970=FACE_OUTER_BOUND('',#1407,.T.);
#971=FACE_OUTER_BOUND('',#1410,.T.);
#972=FACE_OUTER_BOUND('',#1413,.T.);
#973=FACE_OUTER_BOUND('',#1414,.T.);
#974=FACE_OUTER_BOUND('',#1415,.T.);
#975=FACE_OUTER_BOUND('',#1416,.T.);
#976=FACE_OUTER_BOUND('',#1418,.T.);
#977=FACE_OUTER_BOUND('',#1419,.T.);
#978=FACE_OUTER_BOUND('',#1422,.T.);
#979=FACE_OUTER_BOUND('',#1423,.T.);
#980=FACE_OUTER_BOUND('',#1425,.T.);
#981=FACE_OUTER_BOUND('',#1426,.T.);
#982=FACE_OUTER_BOUND('',#1427,.T.);
#983=FACE_OUTER_BOUND('',#1428,.T.);
#984=FACE_OUTER_BOUND('',#1429,.T.);
#985=FACE_OUTER_BOUND('',#1430,.T.);
#986=FACE_OUTER_BOUND('',#1431,.T.);
#987=FACE_OUTER_BOUND('',#1433,.T.);
#988=FACE_OUTER_BOUND('',#1434,.T.);
#989=FACE_OUTER_BOUND('',#1436,.T.);
#990=FACE_OUTER_BOUND('',#1437,.T.);
#991=FACE_OUTER_BOUND('',#1440,.T.);
#992=FACE_OUTER_BOUND('',#1441,.T.);
#993=FACE_OUTER_BOUND('',#1442,.T.);
#994=FACE_OUTER_BOUND('',#1443,.T.);
#995=FACE_OUTER_BOUND('',#1444,.T.);
#996=FACE_OUTER_BOUND('',#1445,.T.);
#997=FACE_OUTER_BOUND('',#1446,.T.);
#998=FACE_OUTER_BOUND('',#1448,.T.);
#999=FACE_OUTER_BOUND('',#1449,.T.);
#1000=FACE_OUTER_BOUND('',#1452,.T.);
#1001=FACE_OUTER_BOUND('',#1453,.T.);
#1002=FACE_OUTER_BOUND('',#1455,.T.);
#1003=FACE_OUTER_BOUND('',#1456,.T.);
#1004=FACE_OUTER_BOUND('',#1457,.T.);
#1005=FACE_OUTER_BOUND('',#1458,.T.);
#1006=FACE_OUTER_BOUND('',#1459,.T.);
#1007=FACE_OUTER_BOUND('',#1460,.T.);
#1008=FACE_OUTER_BOUND('',#1461,.T.);
#1009=FACE_OUTER_BOUND('',#1463,.T.);
#1010=FACE_OUTER_BOUND('',#1464,.T.);
#1011=FACE_OUTER_BOUND('',#1466,.T.);
#1012=FACE_OUTER_BOUND('',#1467,.T.);
#1013=FACE_OUTER_BOUND('',#1470,.T.);
#1014=FACE_OUTER_BOUND('',#1471,.T.);
#1015=FACE_OUTER_BOUND('',#1472,.T.);
#1016=FACE_OUTER_BOUND('',#1473,.T.);
#1017=FACE_OUTER_BOUND('',#1474,.T.);
#1018=FACE_OUTER_BOUND('',#1475,.T.);
#1019=FACE_OUTER_BOUND('',#1476,.T.);
#1020=FACE_OUTER_BOUND('',#1477,.T.);
#1021=FACE_OUTER_BOUND('',#1478,.T.);
#1022=FACE_OUTER_BOUND('',#1479,.T.);
#1023=FACE_OUTER_BOUND('',#1480,.T.);
#1024=FACE_OUTER_BOUND('',#1481,.T.);
#1025=FACE_OUTER_BOUND('',#1483,.T.);
#1026=FACE_OUTER_BOUND('',#1485,.T.);
#1027=FACE_OUTER_BOUND('',#1486,.T.);
#1028=FACE_OUTER_BOUND('',#1487,.T.);
#1029=FACE_OUTER_BOUND('',#1488,.T.);
#1030=FACE_OUTER_BOUND('',#1489,.T.);
#1031=FACE_OUTER_BOUND('',#1490,.T.);
#1032=FACE_OUTER_BOUND('',#1491,.T.);
#1033=FACE_OUTER_BOUND('',#1492,.T.);
#1034=FACE_OUTER_BOUND('',#1493,.T.);
#1035=FACE_OUTER_BOUND('',#1495,.T.);
#1036=FACE_OUTER_BOUND('',#1497,.T.);
#1037=FACE_OUTER_BOUND('',#1498,.T.);
#1038=FACE_OUTER_BOUND('',#1499,.T.);
#1039=FACE_OUTER_BOUND('',#1500,.T.);
#1040=FACE_OUTER_BOUND('',#1501,.T.);
#1041=FACE_OUTER_BOUND('',#1502,.T.);
#1042=FACE_OUTER_BOUND('',#1503,.T.);
#1043=FACE_OUTER_BOUND('',#1504,.T.);
#1044=FACE_OUTER_BOUND('',#1505,.T.);
#1045=FACE_OUTER_BOUND('',#1506,.T.);
#1046=FACE_OUTER_BOUND('',#1515,.T.);
#1047=FACE_OUTER_BOUND('',#1516,.T.);
#1048=FACE_OUTER_BOUND('',#1525,.T.);
#1049=FACE_OUTER_BOUND('',#1526,.T.);
#1050=FACE_OUTER_BOUND('',#1527,.T.);
#1051=FACE_OUTER_BOUND('',#1528,.T.);
#1052=FACE_OUTER_BOUND('',#1529,.T.);
#1053=FACE_OUTER_BOUND('',#1530,.T.);
#1054=FACE_OUTER_BOUND('',#1531,.T.);
#1055=FACE_OUTER_BOUND('',#1532,.T.);
#1056=FACE_OUTER_BOUND('',#1535,.T.);
#1057=FACE_OUTER_BOUND('',#1536,.T.);
#1058=FACE_OUTER_BOUND('',#1539,.T.);
#1059=FACE_OUTER_BOUND('',#1540,.T.);
#1060=FACE_OUTER_BOUND('',#1541,.T.);
#1061=FACE_OUTER_BOUND('',#1542,.T.);
#1062=FACE_OUTER_BOUND('',#1543,.T.);
#1063=FACE_OUTER_BOUND('',#1544,.T.);
#1064=FACE_OUTER_BOUND('',#1545,.T.);
#1065=FACE_OUTER_BOUND('',#1547,.T.);
#1066=FACE_OUTER_BOUND('',#1548,.T.);
#1067=FACE_OUTER_BOUND('',#1549,.T.);
#1068=FACE_OUTER_BOUND('',#1550,.T.);
#1069=FACE_OUTER_BOUND('',#1552,.T.);
#1070=FACE_OUTER_BOUND('',#1553,.T.);
#1071=FACE_OUTER_BOUND('',#1555,.T.);
#1072=FACE_OUTER_BOUND('',#1556,.T.);
#1073=FACE_OUTER_BOUND('',#1557,.T.);
#1074=FACE_OUTER_BOUND('',#1558,.T.);
#1075=FACE_OUTER_BOUND('',#1559,.T.);
#1076=FACE_OUTER_BOUND('',#1560,.T.);
#1077=FACE_OUTER_BOUND('',#1562,.T.);
#1078=FACE_OUTER_BOUND('',#1563,.T.);
#1079=FACE_OUTER_BOUND('',#1564,.T.);
#1080=FACE_OUTER_BOUND('',#1565,.T.);
#1081=FACE_OUTER_BOUND('',#1567,.T.);
#1082=FACE_OUTER_BOUND('',#1568,.T.);
#1083=FACE_OUTER_BOUND('',#1570,.T.);
#1084=FACE_OUTER_BOUND('',#1571,.T.);
#1085=FACE_OUTER_BOUND('',#1572,.T.);
#1086=FACE_OUTER_BOUND('',#1573,.T.);
#1087=FACE_OUTER_BOUND('',#1575,.T.);
#1088=FACE_OUTER_BOUND('',#1576,.T.);
#1089=FACE_OUTER_BOUND('',#1578,.T.);
#1090=FACE_OUTER_BOUND('',#1579,.T.);
#1091=FACE_OUTER_BOUND('',#1580,.T.);
#1092=FACE_OUTER_BOUND('',#1581,.T.);
#1093=FACE_OUTER_BOUND('',#1582,.T.);
#1094=FACE_OUTER_BOUND('',#1584,.T.);
#1095=FACE_OUTER_BOUND('',#1585,.T.);
#1096=FACE_OUTER_BOUND('',#1587,.T.);
#1097=FACE_OUTER_BOUND('',#1588,.T.);
#1098=FACE_OUTER_BOUND('',#1589,.T.);
#1099=FACE_OUTER_BOUND('',#1590,.T.);
#1100=FACE_OUTER_BOUND('',#1591,.T.);
#1101=FACE_OUTER_BOUND('',#1592,.T.);
#1102=FACE_OUTER_BOUND('',#1593,.T.);
#1103=FACE_OUTER_BOUND('',#1594,.T.);
#1104=FACE_OUTER_BOUND('',#1595,.T.);
#1105=FACE_OUTER_BOUND('',#1596,.T.);
#1106=FACE_OUTER_BOUND('',#1597,.T.);
#1107=FACE_OUTER_BOUND('',#1598,.T.);
#1108=FACE_OUTER_BOUND('',#1599,.T.);
#1109=FACE_OUTER_BOUND('',#1600,.T.);
#1110=FACE_OUTER_BOUND('',#1601,.T.);
#1111=FACE_OUTER_BOUND('',#1602,.T.);
#1112=FACE_OUTER_BOUND('',#1603,.T.);
#1113=FACE_OUTER_BOUND('',#1604,.T.);
#1114=FACE_OUTER_BOUND('',#1605,.T.);
#1115=FACE_OUTER_BOUND('',#1606,.T.);
#1116=FACE_OUTER_BOUND('',#1607,.T.);
#1117=FACE_OUTER_BOUND('',#1608,.T.);
#1118=FACE_OUTER_BOUND('',#1609,.T.);
#1119=FACE_OUTER_BOUND('',#1610,.T.);
#1120=FACE_OUTER_BOUND('',#1611,.T.);
#1121=FACE_OUTER_BOUND('',#1612,.T.);
#1122=FACE_OUTER_BOUND('',#1613,.T.);
#1123=FACE_OUTER_BOUND('',#1614,.T.);
#1124=FACE_OUTER_BOUND('',#1615,.T.);
#1125=FACE_OUTER_BOUND('',#1616,.T.);
#1126=FACE_OUTER_BOUND('',#1617,.T.);
#1127=FACE_OUTER_BOUND('',#1618,.T.);
#1128=FACE_OUTER_BOUND('',#1619,.T.);
#1129=FACE_OUTER_BOUND('',#1620,.T.);
#1130=FACE_OUTER_BOUND('',#1621,.T.);
#1131=FACE_OUTER_BOUND('',#1622,.T.);
#1132=FACE_OUTER_BOUND('',#1623,.T.);
#1133=FACE_OUTER_BOUND('',#1624,.T.);
#1134=FACE_OUTER_BOUND('',#1625,.T.);
#1135=FACE_OUTER_BOUND('',#1626,.T.);
#1136=FACE_OUTER_BOUND('',#1627,.T.);
#1137=FACE_OUTER_BOUND('',#1628,.T.);
#1138=FACE_OUTER_BOUND('',#1629,.T.);
#1139=FACE_OUTER_BOUND('',#1630,.T.);
#1140=FACE_OUTER_BOUND('',#1631,.T.);
#1141=FACE_OUTER_BOUND('',#1632,.T.);
#1142=FACE_OUTER_BOUND('',#1633,.T.);
#1143=FACE_OUTER_BOUND('',#1634,.T.);
#1144=FACE_OUTER_BOUND('',#1636,.T.);
#1145=FACE_OUTER_BOUND('',#1638,.T.);
#1146=FACE_OUTER_BOUND('',#1639,.T.);
#1147=FACE_OUTER_BOUND('',#1640,.T.);
#1148=FACE_OUTER_BOUND('',#1641,.T.);
#1149=FACE_OUTER_BOUND('',#1642,.T.);
#1150=FACE_OUTER_BOUND('',#1644,.T.);
#1151=FACE_OUTER_BOUND('',#1645,.T.);
#1152=FACE_OUTER_BOUND('',#1646,.T.);
#1153=FACE_OUTER_BOUND('',#1647,.T.);
#1154=FACE_OUTER_BOUND('',#1648,.T.);
#1155=FACE_OUTER_BOUND('',#1649,.T.);
#1156=FACE_OUTER_BOUND('',#1650,.T.);
#1157=FACE_OUTER_BOUND('',#1651,.T.);
#1158=FACE_OUTER_BOUND('',#1652,.T.);
#1159=FACE_OUTER_BOUND('',#1653,.T.);
#1160=FACE_OUTER_BOUND('',#1654,.T.);
#1161=FACE_OUTER_BOUND('',#1655,.T.);
#1162=FACE_OUTER_BOUND('',#1656,.T.);
#1163=FACE_OUTER_BOUND('',#1657,.T.);
#1164=FACE_OUTER_BOUND('',#1659,.T.);
#1165=FACE_OUTER_BOUND('',#1660,.T.);
#1166=FACE_OUTER_BOUND('',#1662,.T.);
#1167=FACE_OUTER_BOUND('',#1663,.T.);
#1168=FACE_OUTER_BOUND('',#1665,.T.);
#1169=FACE_OUTER_BOUND('',#1666,.T.);
#1170=FACE_OUTER_BOUND('',#1668,.T.);
#1171=FACE_OUTER_BOUND('',#1669,.T.);
#1172=FACE_OUTER_BOUND('',#1670,.T.);
#1173=FACE_OUTER_BOUND('',#1671,.T.);
#1174=FACE_OUTER_BOUND('',#1672,.T.);
#1175=FACE_OUTER_BOUND('',#1673,.T.);
#1176=FACE_OUTER_BOUND('',#1674,.T.);
#1177=FACE_OUTER_BOUND('',#1675,.T.);
#1178=FACE_OUTER_BOUND('',#1676,.T.);
#1179=FACE_OUTER_BOUND('',#1681,.T.);
#1180=FACE_OUTER_BOUND('',#1682,.T.);
#1181=FACE_OUTER_BOUND('',#1683,.T.);
#1182=FACE_OUTER_BOUND('',#1684,.T.);
#1183=FACE_OUTER_BOUND('',#1685,.T.);
#1184=FACE_OUTER_BOUND('',#1686,.T.);
#1185=FACE_OUTER_BOUND('',#1691,.T.);
#1186=FACE_OUTER_BOUND('',#1692,.T.);
#1187=FACE_OUTER_BOUND('',#1693,.T.);
#1188=FACE_OUTER_BOUND('',#1694,.T.);
#1189=FACE_OUTER_BOUND('',#1695,.T.);
#1190=FACE_OUTER_BOUND('',#1696,.T.);
#1191=FACE_OUTER_BOUND('',#1698,.T.);
#1192=FACE_OUTER_BOUND('',#1699,.T.);
#1193=FACE_OUTER_BOUND('',#1700,.T.);
#1194=FACE_OUTER_BOUND('',#1701,.T.);
#1195=FACE_OUTER_BOUND('',#1702,.T.);
#1196=FACE_OUTER_BOUND('',#1703,.T.);
#1197=FACE_OUTER_BOUND('',#1704,.T.);
#1198=FACE_OUTER_BOUND('',#1705,.T.);
#1199=FACE_OUTER_BOUND('',#1706,.T.);
#1200=FACE_OUTER_BOUND('',#1707,.T.);
#1201=FACE_OUTER_BOUND('',#1708,.T.);
#1202=FACE_OUTER_BOUND('',#1709,.T.);
#1203=FACE_OUTER_BOUND('',#1710,.T.);
#1204=FACE_OUTER_BOUND('',#1711,.T.);
#1205=FACE_OUTER_BOUND('',#1713,.T.);
#1206=FACE_OUTER_BOUND('',#1714,.T.);
#1207=FACE_OUTER_BOUND('',#1716,.T.);
#1208=FACE_OUTER_BOUND('',#1717,.T.);
#1209=FACE_OUTER_BOUND('',#1718,.T.);
#1210=FACE_OUTER_BOUND('',#1719,.T.);
#1211=FACE_OUTER_BOUND('',#1720,.T.);
#1212=FACE_OUTER_BOUND('',#1721,.T.);
#1213=FACE_OUTER_BOUND('',#1722,.T.);
#1214=FACE_OUTER_BOUND('',#1723,.T.);
#1215=FACE_OUTER_BOUND('',#1724,.T.);
#1216=FACE_OUTER_BOUND('',#1726,.T.);
#1217=FACE_OUTER_BOUND('',#1727,.T.);
#1218=FACE_OUTER_BOUND('',#1728,.T.);
#1219=FACE_OUTER_BOUND('',#1729,.T.);
#1220=FACE_OUTER_BOUND('',#1730,.T.);
#1221=FACE_OUTER_BOUND('',#1731,.T.);
#1222=FACE_OUTER_BOUND('',#1732,.T.);
#1223=FACE_OUTER_BOUND('',#1734,.T.);
#1224=FACE_OUTER_BOUND('',#1735,.T.);
#1225=FACE_OUTER_BOUND('',#1736,.T.);
#1226=FACE_OUTER_BOUND('',#1737,.T.);
#1227=FACE_OUTER_BOUND('',#1738,.T.);
#1228=FACE_OUTER_BOUND('',#1739,.T.);
#1229=FACE_OUTER_BOUND('',#1740,.T.);
#1230=FACE_OUTER_BOUND('',#1741,.T.);
#1231=FACE_OUTER_BOUND('',#1742,.T.);
#1232=FACE_OUTER_BOUND('',#1743,.T.);
#1233=FACE_OUTER_BOUND('',#1744,.T.);
#1234=FACE_OUTER_BOUND('',#1745,.T.);
#1235=FACE_OUTER_BOUND('',#1752,.T.);
#1236=FACE_OUTER_BOUND('',#1753,.T.);
#1237=FACE_OUTER_BOUND('',#1754,.T.);
#1238=FACE_OUTER_BOUND('',#1755,.T.);
#1239=FACE_OUTER_BOUND('',#1756,.T.);
#1240=FACE_OUTER_BOUND('',#1757,.T.);
#1241=FACE_OUTER_BOUND('',#1764,.T.);
#1242=FACE_OUTER_BOUND('',#1765,.T.);
#1243=FACE_OUTER_BOUND('',#1766,.T.);
#1244=FACE_OUTER_BOUND('',#1767,.T.);
#1245=FACE_OUTER_BOUND('',#1768,.T.);
#1246=FACE_OUTER_BOUND('',#1769,.T.);
#1247=FACE_OUTER_BOUND('',#1771,.T.);
#1248=FACE_OUTER_BOUND('',#1772,.T.);
#1249=FACE_OUTER_BOUND('',#1773,.T.);
#1250=FACE_OUTER_BOUND('',#1774,.T.);
#1251=FACE_OUTER_BOUND('',#1776,.T.);
#1252=FACE_OUTER_BOUND('',#1777,.T.);
#1253=FACE_OUTER_BOUND('',#1778,.T.);
#1254=FACE_OUTER_BOUND('',#1779,.T.);
#1255=FACE_OUTER_BOUND('',#1780,.T.);
#1256=FACE_OUTER_BOUND('',#1781,.T.);
#1257=FACE_OUTER_BOUND('',#1782,.T.);
#1258=FACE_OUTER_BOUND('',#1783,.T.);
#1259=FACE_OUTER_BOUND('',#1784,.T.);
#1260=FACE_OUTER_BOUND('',#1785,.T.);
#1261=FACE_OUTER_BOUND('',#1786,.T.);
#1262=FACE_OUTER_BOUND('',#1787,.T.);
#1263=FACE_OUTER_BOUND('',#1788,.T.);
#1264=FACE_OUTER_BOUND('',#1789,.T.);
#1265=FACE_OUTER_BOUND('',#1790,.T.);
#1266=FACE_OUTER_BOUND('',#1791,.T.);
#1267=FACE_OUTER_BOUND('',#1792,.T.);
#1268=FACE_OUTER_BOUND('',#1797,.T.);
#1269=FACE_OUTER_BOUND('',#1798,.T.);
#1270=FACE_OUTER_BOUND('',#1799,.T.);
#1271=FACE_OUTER_BOUND('',#1800,.T.);
#1272=FACE_OUTER_BOUND('',#1801,.T.);
#1273=FACE_OUTER_BOUND('',#1802,.T.);
#1274=FACE_OUTER_BOUND('',#1803,.T.);
#1275=FACE_OUTER_BOUND('',#1804,.T.);
#1276=FACE_OUTER_BOUND('',#1805,.T.);
#1277=FACE_OUTER_BOUND('',#1806,.T.);
#1278=FACE_OUTER_BOUND('',#1807,.T.);
#1279=FACE_OUTER_BOUND('',#1808,.T.);
#1280=FACE_OUTER_BOUND('',#1809,.T.);
#1281=FACE_OUTER_BOUND('',#1810,.T.);
#1282=FACE_OUTER_BOUND('',#1811,.T.);
#1283=FACE_OUTER_BOUND('',#1812,.T.);
#1284=FACE_OUTER_BOUND('',#1813,.T.);
#1285=FACE_OUTER_BOUND('',#1814,.T.);
#1286=FACE_OUTER_BOUND('',#1815,.T.);
#1287=FACE_OUTER_BOUND('',#1816,.T.);
#1288=FACE_OUTER_BOUND('',#1817,.T.);
#1289=FACE_OUTER_BOUND('',#1818,.T.);
#1290=FACE_OUTER_BOUND('',#1819,.T.);
#1291=FACE_OUTER_BOUND('',#1820,.T.);
#1292=FACE_OUTER_BOUND('',#1821,.T.);
#1293=FACE_OUTER_BOUND('',#1822,.T.);
#1294=FACE_OUTER_BOUND('',#1823,.T.);
#1295=FACE_OUTER_BOUND('',#1824,.T.);
#1296=FACE_OUTER_BOUND('',#1825,.T.);
#1297=FACE_OUTER_BOUND('',#1826,.T.);
#1298=FACE_OUTER_BOUND('',#1827,.T.);
#1299=FACE_OUTER_BOUND('',#1828,.T.);
#1300=FACE_OUTER_BOUND('',#1829,.T.);
#1301=FACE_OUTER_BOUND('',#1830,.T.);
#1302=FACE_OUTER_BOUND('',#1831,.T.);
#1303=FACE_OUTER_BOUND('',#1832,.T.);
#1304=FACE_OUTER_BOUND('',#1833,.T.);
#1305=FACE_OUTER_BOUND('',#1834,.T.);
#1306=FACE_OUTER_BOUND('',#1835,.T.);
#1307=FACE_OUTER_BOUND('',#1836,.T.);
#1308=FACE_OUTER_BOUND('',#1837,.T.);
#1309=FACE_OUTER_BOUND('',#1838,.T.);
#1310=FACE_OUTER_BOUND('',#1840,.T.);
#1311=FACE_OUTER_BOUND('',#1841,.T.);
#1312=FACE_OUTER_BOUND('',#1842,.T.);
#1313=FACE_OUTER_BOUND('',#1843,.T.);
#1314=FACE_OUTER_BOUND('',#1844,.T.);
#1315=FACE_OUTER_BOUND('',#1845,.T.);
#1316=FACE_OUTER_BOUND('',#1846,.T.);
#1317=FACE_OUTER_BOUND('',#1848,.T.);
#1318=FACE_OUTER_BOUND('',#1849,.T.);
#1319=FACE_OUTER_BOUND('',#1850,.T.);
#1320=FACE_OUTER_BOUND('',#1851,.T.);
#1321=FACE_OUTER_BOUND('',#1852,.T.);
#1322=FACE_OUTER_BOUND('',#1853,.T.);
#1323=FACE_OUTER_BOUND('',#1854,.T.);
#1324=FACE_OUTER_BOUND('',#1855,.T.);
#1325=FACE_OUTER_BOUND('',#1856,.T.);
#1326=FACE_OUTER_BOUND('',#1857,.T.);
#1327=FACE_OUTER_BOUND('',#1858,.T.);
#1328=FACE_OUTER_BOUND('',#1859,.T.);
#1329=EDGE_LOOP('',(#5186,#5187,#5188,#5189));
#1330=EDGE_LOOP('',(#5190,#5191,#5192,#5193));
#1331=EDGE_LOOP('',(#5194,#5195,#5196,#5197));
#1332=EDGE_LOOP('',(#5198,#5199,#5200,#5201));
#1333=EDGE_LOOP('',(#5202,#5203,#5204,#5205));
#1334=EDGE_LOOP('',(#5206,#5207,#5208,#5209));
#1335=EDGE_LOOP('',(#5210,#5211,#5212,#5213));
#1336=EDGE_LOOP('',(#5214,#5215,#5216,#5217));
#1337=EDGE_LOOP('',(#5218,#5219,#5220,#5221));
#1338=EDGE_LOOP('',(#5222));
#1339=EDGE_LOOP('',(#5223));
#1340=EDGE_LOOP('',(#5224));
#1341=EDGE_LOOP('',(#5225));
#1342=EDGE_LOOP('',(#5226,#5227,#5228,#5229));
#1343=EDGE_LOOP('',(#5230));
#1344=EDGE_LOOP('',(#5231));
#1345=EDGE_LOOP('',(#5232));
#1346=EDGE_LOOP('',(#5233));
#1347=EDGE_LOOP('',(#5234,#5235,#5236,#5237));
#1348=EDGE_LOOP('',(#5238,#5239,#5240,#5241));
#1349=EDGE_LOOP('',(#5242,#5243,#5244,#5245));
#1350=EDGE_LOOP('',(#5246,#5247,#5248,#5249));
#1351=EDGE_LOOP('',(#5250,#5251,#5252,#5253));
#1352=EDGE_LOOP('',(#5254,#5255,#5256,#5257));
#1353=EDGE_LOOP('',(#5258,#5259,#5260,#5261));
#1354=EDGE_LOOP('',(#5262,#5263,#5264,#5265));
#1355=EDGE_LOOP('',(#5266,#5267,#5268,#5269));
#1356=EDGE_LOOP('',(#5270,#5271,#5272,#5273));
#1357=EDGE_LOOP('',(#5274,#5275,#5276,#5277));
#1358=EDGE_LOOP('',(#5278,#5279,#5280,#5281));
#1359=EDGE_LOOP('',(#5282,#5283,#5284,#5285));
#1360=EDGE_LOOP('',(#5286,#5287,#5288,#5289));
#1361=EDGE_LOOP('',(#5290));
#1362=EDGE_LOOP('',(#5291));
#1363=EDGE_LOOP('',(#5292));
#1364=EDGE_LOOP('',(#5293));
#1365=EDGE_LOOP('',(#5294,#5295,#5296,#5297));
#1366=EDGE_LOOP('',(#5298,#5299,#5300,#5301));
#1367=EDGE_LOOP('',(#5302));
#1368=EDGE_LOOP('',(#5303));
#1369=EDGE_LOOP('',(#5304));
#1370=EDGE_LOOP('',(#5305));
#1371=EDGE_LOOP('',(#5306,#5307,#5308,#5309));
#1372=EDGE_LOOP('',(#5310,#5311,#5312,#5313));
#1373=EDGE_LOOP('',(#5314,#5315,#5316,#5317));
#1374=EDGE_LOOP('',(#5318,#5319,#5320,#5321));
#1375=EDGE_LOOP('',(#5322,#5323,#5324,#5325));
#1376=EDGE_LOOP('',(#5326,#5327,#5328,#5329));
#1377=EDGE_LOOP('',(#5330,#5331,#5332,#5333));
#1378=EDGE_LOOP('',(#5334,#5335,#5336,#5337));
#1379=EDGE_LOOP('',(#5338,#5339,#5340,#5341));
#1380=EDGE_LOOP('',(#5342,#5343,#5344,#5345));
#1381=EDGE_LOOP('',(#5346,#5347,#5348,#5349));
#1382=EDGE_LOOP('',(#5350,#5351,#5352,#5353));
#1383=EDGE_LOOP('',(#5354,#5355,#5356,#5357));
#1384=EDGE_LOOP('',(#5358,#5359,#5360,#5361));
#1385=EDGE_LOOP('',(#5362,#5363,#5364,#5365));
#1386=EDGE_LOOP('',(#5366,#5367,#5368,#5369));
#1387=EDGE_LOOP('',(#5370,#5371,#5372,#5373));
#1388=EDGE_LOOP('',(#5374,#5375,#5376,#5377));
#1389=EDGE_LOOP('',(#5378,#5379,#5380,#5381));
#1390=EDGE_LOOP('',(#5382,#5383,#5384,#5385));
#1391=EDGE_LOOP('',(#5386,#5387,#5388,#5389));
#1392=EDGE_LOOP('',(#5390,#5391,#5392,#5393));
#1393=EDGE_LOOP('',(#5394,#5395,#5396,#5397));
#1394=EDGE_LOOP('',(#5398,#5399,#5400,#5401));
#1395=EDGE_LOOP('',(#5402,#5403,#5404,#5405));
#1396=EDGE_LOOP('',(#5406));
#1397=EDGE_LOOP('',(#5407));
#1398=EDGE_LOOP('',(#5408,#5409,#5410,#5411));
#1399=EDGE_LOOP('',(#5412));
#1400=EDGE_LOOP('',(#5413));
#1401=EDGE_LOOP('',(#5414,#5415,#5416,#5417));
#1402=EDGE_LOOP('',(#5418,#5419,#5420,#5421));
#1403=EDGE_LOOP('',(#5422,#5423,#5424,#5425));
#1404=EDGE_LOOP('',(#5426,#5427,#5428,#5429));
#1405=EDGE_LOOP('',(#5430,#5431,#5432,#5433));
#1406=EDGE_LOOP('',(#5434,#5435,#5436,#5437));
#1407=EDGE_LOOP('',(#5438,#5439,#5440,#5441));
#1408=EDGE_LOOP('',(#5442));
#1409=EDGE_LOOP('',(#5443));
#1410=EDGE_LOOP('',(#5444,#5445,#5446,#5447));
#1411=EDGE_LOOP('',(#5448));
#1412=EDGE_LOOP('',(#5449));
#1413=EDGE_LOOP('',(#5450,#5451,#5452,#5453));
#1414=EDGE_LOOP('',(#5454));
#1415=EDGE_LOOP('',(#5455,#5456,#5457,#5458));
#1416=EDGE_LOOP('',(#5459));
#1417=EDGE_LOOP('',(#5460));
#1418=EDGE_LOOP('',(#5461,#5462,#5463,#5464));
#1419=EDGE_LOOP('',(#5465,#5466,#5467,#5468));
#1420=EDGE_LOOP('',(#5469));
#1421=EDGE_LOOP('',(#5470));
#1422=EDGE_LOOP('',(#5471,#5472,#5473,#5474));
#1423=EDGE_LOOP('',(#5475,#5476,#5477,#5478));
#1424=EDGE_LOOP('',(#5479));
#1425=EDGE_LOOP('',(#5480,#5481,#5482,#5483));
#1426=EDGE_LOOP('',(#5484,#5485,#5486,#5487));
#1427=EDGE_LOOP('',(#5488,#5489,#5490,#5491));
#1428=EDGE_LOOP('',(#5492,#5493,#5494,#5495));
#1429=EDGE_LOOP('',(#5496));
#1430=EDGE_LOOP('',(#5497,#5498,#5499,#5500));
#1431=EDGE_LOOP('',(#5501));
#1432=EDGE_LOOP('',(#5502));
#1433=EDGE_LOOP('',(#5503,#5504,#5505,#5506));
#1434=EDGE_LOOP('',(#5507,#5508,#5509,#5510));
#1435=EDGE_LOOP('',(#5511));
#1436=EDGE_LOOP('',(#5512,#5513,#5514,#5515));
#1437=EDGE_LOOP('',(#5516,#5517,#5518,#5519));
#1438=EDGE_LOOP('',(#5520));
#1439=EDGE_LOOP('',(#5521));
#1440=EDGE_LOOP('',(#5522,#5523,#5524,#5525));
#1441=EDGE_LOOP('',(#5526,#5527,#5528,#5529));
#1442=EDGE_LOOP('',(#5530,#5531,#5532,#5533));
#1443=EDGE_LOOP('',(#5534,#5535,#5536,#5537));
#1444=EDGE_LOOP('',(#5538));
#1445=EDGE_LOOP('',(#5539,#5540,#5541,#5542));
#1446=EDGE_LOOP('',(#5543));
#1447=EDGE_LOOP('',(#5544));
#1448=EDGE_LOOP('',(#5545,#5546,#5547,#5548));
#1449=EDGE_LOOP('',(#5549,#5550,#5551,#5552));
#1450=EDGE_LOOP('',(#5553));
#1451=EDGE_LOOP('',(#5554));
#1452=EDGE_LOOP('',(#5555,#5556,#5557,#5558));
#1453=EDGE_LOOP('',(#5559,#5560,#5561,#5562));
#1454=EDGE_LOOP('',(#5563));
#1455=EDGE_LOOP('',(#5564,#5565,#5566,#5567));
#1456=EDGE_LOOP('',(#5568,#5569,#5570,#5571));
#1457=EDGE_LOOP('',(#5572,#5573,#5574,#5575));
#1458=EDGE_LOOP('',(#5576,#5577,#5578,#5579));
#1459=EDGE_LOOP('',(#5580));
#1460=EDGE_LOOP('',(#5581,#5582,#5583,#5584));
#1461=EDGE_LOOP('',(#5585));
#1462=EDGE_LOOP('',(#5586));
#1463=EDGE_LOOP('',(#5587,#5588,#5589,#5590));
#1464=EDGE_LOOP('',(#5591,#5592,#5593,#5594));
#1465=EDGE_LOOP('',(#5595));
#1466=EDGE_LOOP('',(#5596,#5597,#5598,#5599));
#1467=EDGE_LOOP('',(#5600,#5601,#5602,#5603));
#1468=EDGE_LOOP('',(#5604));
#1469=EDGE_LOOP('',(#5605));
#1470=EDGE_LOOP('',(#5606,#5607,#5608,#5609));
#1471=EDGE_LOOP('',(#5610,#5611,#5612,#5613));
#1472=EDGE_LOOP('',(#5614,#5615,#5616,#5617));
#1473=EDGE_LOOP('',(#5618,#5619,#5620,#5621));
#1474=EDGE_LOOP('',(#5622,#5623,#5624,#5625));
#1475=EDGE_LOOP('',(#5626,#5627,#5628,#5629));
#1476=EDGE_LOOP('',(#5630,#5631,#5632,#5633));
#1477=EDGE_LOOP('',(#5634,#5635,#5636,#5637));
#1478=EDGE_LOOP('',(#5638,#5639,#5640,#5641));
#1479=EDGE_LOOP('',(#5642,#5643,#5644,#5645));
#1480=EDGE_LOOP('',(#5646,#5647,#5648,#5649));
#1481=EDGE_LOOP('',(#5650,#5651,#5652,#5653));
#1482=EDGE_LOOP('',(#5654,#5655,#5656,#5657));
#1483=EDGE_LOOP('',(#5658,#5659,#5660,#5661));
#1484=EDGE_LOOP('',(#5662,#5663,#5664,#5665));
#1485=EDGE_LOOP('',(#5666,#5667,#5668,#5669));
#1486=EDGE_LOOP('',(#5670,#5671,#5672,#5673));
#1487=EDGE_LOOP('',(#5674,#5675,#5676,#5677));
#1488=EDGE_LOOP('',(#5678,#5679,#5680,#5681));
#1489=EDGE_LOOP('',(#5682,#5683,#5684,#5685));
#1490=EDGE_LOOP('',(#5686,#5687,#5688,#5689));
#1491=EDGE_LOOP('',(#5690,#5691,#5692,#5693));
#1492=EDGE_LOOP('',(#5694,#5695,#5696,#5697));
#1493=EDGE_LOOP('',(#5698,#5699,#5700,#5701));
#1494=EDGE_LOOP('',(#5702,#5703,#5704,#5705));
#1495=EDGE_LOOP('',(#5706,#5707,#5708,#5709));
#1496=EDGE_LOOP('',(#5710,#5711,#5712,#5713));
#1497=EDGE_LOOP('',(#5714,#5715,#5716,#5717));
#1498=EDGE_LOOP('',(#5718,#5719,#5720,#5721));
#1499=EDGE_LOOP('',(#5722,#5723,#5724,#5725));
#1500=EDGE_LOOP('',(#5726,#5727,#5728,#5729));
#1501=EDGE_LOOP('',(#5730,#5731,#5732,#5733));
#1502=EDGE_LOOP('',(#5734,#5735,#5736,#5737));
#1503=EDGE_LOOP('',(#5738,#5739,#5740,#5741));
#1504=EDGE_LOOP('',(#5742,#5743,#5744,#5745));
#1505=EDGE_LOOP('',(#5746,#5747,#5748,#5749));
#1506=EDGE_LOOP('',(#5750,#5751,#5752,#5753));
#1507=EDGE_LOOP('',(#5754));
#1508=EDGE_LOOP('',(#5755));
#1509=EDGE_LOOP('',(#5756));
#1510=EDGE_LOOP('',(#5757));
#1511=EDGE_LOOP('',(#5758));
#1512=EDGE_LOOP('',(#5759));
#1513=EDGE_LOOP('',(#5760));
#1514=EDGE_LOOP('',(#5761));
#1515=EDGE_LOOP('',(#5762,#5763,#5764,#5765));
#1516=EDGE_LOOP('',(#5766,#5767,#5768,#5769));
#1517=EDGE_LOOP('',(#5770));
#1518=EDGE_LOOP('',(#5771));
#1519=EDGE_LOOP('',(#5772));
#1520=EDGE_LOOP('',(#5773));
#1521=EDGE_LOOP('',(#5774));
#1522=EDGE_LOOP('',(#5775));
#1523=EDGE_LOOP('',(#5776));
#1524=EDGE_LOOP('',(#5777));
#1525=EDGE_LOOP('',(#5778,#5779,#5780,#5781));
#1526=EDGE_LOOP('',(#5782,#5783,#5784,#5785));
#1527=EDGE_LOOP('',(#5786,#5787,#5788,#5789));
#1528=EDGE_LOOP('',(#5790,#5791,#5792,#5793));
#1529=EDGE_LOOP('',(#5794,#5795,#5796,#5797));
#1530=EDGE_LOOP('',(#5798,#5799,#5800,#5801));
#1531=EDGE_LOOP('',(#5802,#5803,#5804,#5805));
#1532=EDGE_LOOP('',(#5806,#5807,#5808,#5809));
#1533=EDGE_LOOP('',(#5810));
#1534=EDGE_LOOP('',(#5811));
#1535=EDGE_LOOP('',(#5812,#5813,#5814,#5815));
#1536=EDGE_LOOP('',(#5816,#5817,#5818,#5819));
#1537=EDGE_LOOP('',(#5820));
#1538=EDGE_LOOP('',(#5821));
#1539=EDGE_LOOP('',(#5822,#5823,#5824,#5825,#5826,#5827));
#1540=EDGE_LOOP('',(#5828,#5829,#5830,#5831,#5832,#5833));
#1541=EDGE_LOOP('',(#5834,#5835,#5836,#5837));
#1542=EDGE_LOOP('',(#5838));
#1543=EDGE_LOOP('',(#5839,#5840,#5841,#5842));
#1544=EDGE_LOOP('',(#5843,#5844,#5845,#5846));
#1545=EDGE_LOOP('',(#5847,#5848,#5849,#5850));
#1546=EDGE_LOOP('',(#5851));
#1547=EDGE_LOOP('',(#5852,#5853,#5854,#5855));
#1548=EDGE_LOOP('',(#5856,#5857,#5858,#5859,#5860,#5861));
#1549=EDGE_LOOP('',(#5862,#5863,#5864,#5865,#5866,#5867));
#1550=EDGE_LOOP('',(#5868,#5869,#5870,#5871));
#1551=EDGE_LOOP('',(#5872));
#1552=EDGE_LOOP('',(#5873,#5874,#5875,#5876));
#1553=EDGE_LOOP('',(#5877,#5878,#5879,#5880,#5881,#5882));
#1554=EDGE_LOOP('',(#5883));
#1555=EDGE_LOOP('',(#5884,#5885,#5886,#5887));
#1556=EDGE_LOOP('',(#5888,#5889,#5890,#5891));
#1557=EDGE_LOOP('',(#5892));
#1558=EDGE_LOOP('',(#5893,#5894,#5895,#5896));
#1559=EDGE_LOOP('',(#5897,#5898,#5899,#5900));
#1560=EDGE_LOOP('',(#5901,#5902,#5903,#5904));
#1561=EDGE_LOOP('',(#5905));
#1562=EDGE_LOOP('',(#5906,#5907,#5908,#5909));
#1563=EDGE_LOOP('',(#5910,#5911,#5912,#5913,#5914,#5915));
#1564=EDGE_LOOP('',(#5916,#5917,#5918,#5919,#5920,#5921));
#1565=EDGE_LOOP('',(#5922,#5923,#5924,#5925));
#1566=EDGE_LOOP('',(#5926));
#1567=EDGE_LOOP('',(#5927,#5928,#5929,#5930));
#1568=EDGE_LOOP('',(#5931,#5932,#5933,#5934,#5935,#5936));
#1569=EDGE_LOOP('',(#5937));
#1570=EDGE_LOOP('',(#5938,#5939,#5940,#5941));
#1571=EDGE_LOOP('',(#5942,#5943,#5944,#5945));
#1572=EDGE_LOOP('',(#5946,#5947,#5948,#5949));
#1573=EDGE_LOOP('',(#5950,#5951,#5952,#5953));
#1574=EDGE_LOOP('',(#5954));
#1575=EDGE_LOOP('',(#5955,#5956,#5957,#5958));
#1576=EDGE_LOOP('',(#5959,#5960,#5961,#5962));
#1577=EDGE_LOOP('',(#5963));
#1578=EDGE_LOOP('',(#5964,#5965,#5966,#5967));
#1579=EDGE_LOOP('',(#5968,#5969,#5970,#5971));
#1580=EDGE_LOOP('',(#5972,#5973,#5974,#5975));
#1581=EDGE_LOOP('',(#5976,#5977,#5978,#5979));
#1582=EDGE_LOOP('',(#5980,#5981,#5982,#5983));
#1583=EDGE_LOOP('',(#5984));
#1584=EDGE_LOOP('',(#5985,#5986,#5987,#5988));
#1585=EDGE_LOOP('',(#5989,#5990,#5991,#5992));
#1586=EDGE_LOOP('',(#5993));
#1587=EDGE_LOOP('',(#5994,#5995,#5996,#5997));
#1588=EDGE_LOOP('',(#5998,#5999,#6000,#6001));
#1589=EDGE_LOOP('',(#6002,#6003,#6004,#6005));
#1590=EDGE_LOOP('',(#6006,#6007,#6008,#6009));
#1591=EDGE_LOOP('',(#6010,#6011,#6012,#6013));
#1592=EDGE_LOOP('',(#6014,#6015,#6016,#6017));
#1593=EDGE_LOOP('',(#6018,#6019,#6020,#6021));
#1594=EDGE_LOOP('',(#6022,#6023,#6024,#6025));
#1595=EDGE_LOOP('',(#6026,#6027,#6028,#6029));
#1596=EDGE_LOOP('',(#6030,#6031,#6032,#6033));
#1597=EDGE_LOOP('',(#6034,#6035,#6036,#6037));
#1598=EDGE_LOOP('',(#6038,#6039,#6040,#6041));
#1599=EDGE_LOOP('',(#6042,#6043,#6044,#6045));
#1600=EDGE_LOOP('',(#6046,#6047,#6048,#6049));
#1601=EDGE_LOOP('',(#6050,#6051,#6052,#6053));
#1602=EDGE_LOOP('',(#6054,#6055,#6056,#6057));
#1603=EDGE_LOOP('',(#6058,#6059,#6060,#6061));
#1604=EDGE_LOOP('',(#6062,#6063,#6064,#6065));
#1605=EDGE_LOOP('',(#6066,#6067,#6068,#6069));
#1606=EDGE_LOOP('',(#6070,#6071,#6072,#6073));
#1607=EDGE_LOOP('',(#6074,#6075,#6076,#6077));
#1608=EDGE_LOOP('',(#6078,#6079,#6080,#6081));
#1609=EDGE_LOOP('',(#6082,#6083,#6084,#6085));
#1610=EDGE_LOOP('',(#6086,#6087,#6088,#6089));
#1611=EDGE_LOOP('',(#6090,#6091,#6092,#6093));
#1612=EDGE_LOOP('',(#6094,#6095,#6096,#6097));
#1613=EDGE_LOOP('',(#6098,#6099,#6100,#6101));
#1614=EDGE_LOOP('',(#6102,#6103,#6104,#6105));
#1615=EDGE_LOOP('',(#6106,#6107,#6108,#6109));
#1616=EDGE_LOOP('',(#6110,#6111,#6112,#6113));
#1617=EDGE_LOOP('',(#6114,#6115,#6116,#6117));
#1618=EDGE_LOOP('',(#6118,#6119,#6120,#6121));
#1619=EDGE_LOOP('',(#6122,#6123,#6124,#6125));
#1620=EDGE_LOOP('',(#6126,#6127,#6128,#6129));
#1621=EDGE_LOOP('',(#6130,#6131,#6132,#6133));
#1622=EDGE_LOOP('',(#6134,#6135,#6136,#6137));
#1623=EDGE_LOOP('',(#6138,#6139,#6140,#6141));
#1624=EDGE_LOOP('',(#6142,#6143,#6144,#6145));
#1625=EDGE_LOOP('',(#6146,#6147,#6148,#6149));
#1626=EDGE_LOOP('',(#6150,#6151,#6152,#6153));
#1627=EDGE_LOOP('',(#6154,#6155,#6156,#6157));
#1628=EDGE_LOOP('',(#6158,#6159,#6160,#6161));
#1629=EDGE_LOOP('',(#6162,#6163,#6164,#6165));
#1630=EDGE_LOOP('',(#6166,#6167,#6168,#6169));
#1631=EDGE_LOOP('',(#6170,#6171,#6172,#6173));
#1632=EDGE_LOOP('',(#6174,#6175,#6176,#6177));
#1633=EDGE_LOOP('',(#6178,#6179,#6180,#6181));
#1634=EDGE_LOOP('',(#6182,#6183,#6184,#6185,#6186,#6187,#6188,#6189,#6190,
#6191,#6192,#6193,#6194,#6195,#6196,#6197,#6198,#6199,#6200,#6201,#6202,
#6203,#6204,#6205,#6206,#6207,#6208,#6209,#6210,#6211,#6212,#6213,#6214,
#6215,#6216,#6217,#6218,#6219,#6220,#6221,#6222,#6223,#6224,#6225));
#1635=EDGE_LOOP('',(#6226));
#1636=EDGE_LOOP('',(#6227,#6228,#6229,#6230,#6231,#6232,#6233,#6234,#6235,
#6236,#6237,#6238,#6239,#6240,#6241,#6242,#6243,#6244,#6245,#6246,#6247,
#6248,#6249,#6250,#6251,#6252,#6253,#6254,#6255,#6256,#6257,#6258,#6259,
#6260,#6261,#6262,#6263,#6264,#6265,#6266,#6267,#6268,#6269,#6270));
#1637=EDGE_LOOP('',(#6271));
#1638=EDGE_LOOP('',(#6272));
#1639=EDGE_LOOP('',(#6273,#6274,#6275,#6276));
#1640=EDGE_LOOP('',(#6277,#6278,#6279,#6280));
#1641=EDGE_LOOP('',(#6281,#6282,#6283,#6284));
#1642=EDGE_LOOP('',(#6285));
#1643=EDGE_LOOP('',(#6286));
#1644=EDGE_LOOP('',(#6287,#6288,#6289,#6290));
#1645=EDGE_LOOP('',(#6291,#6292,#6293,#6294));
#1646=EDGE_LOOP('',(#6295,#6296,#6297,#6298));
#1647=EDGE_LOOP('',(#6299));
#1648=EDGE_LOOP('',(#6300,#6301,#6302,#6303));
#1649=EDGE_LOOP('',(#6304,#6305,#6306,#6307));
#1650=EDGE_LOOP('',(#6308,#6309,#6310,#6311));
#1651=EDGE_LOOP('',(#6312,#6313,#6314,#6315));
#1652=EDGE_LOOP('',(#6316,#6317,#6318,#6319));
#1653=EDGE_LOOP('',(#6320,#6321,#6322,#6323));
#1654=EDGE_LOOP('',(#6324,#6325,#6326,#6327,#6328,#6329));
#1655=EDGE_LOOP('',(#6330,#6331,#6332,#6333,#6334,#6335));
#1656=EDGE_LOOP('',(#6336,#6337,#6338,#6339));
#1657=EDGE_LOOP('',(#6340));
#1658=EDGE_LOOP('',(#6341));
#1659=EDGE_LOOP('',(#6342,#6343,#6344,#6345));
#1660=EDGE_LOOP('',(#6346));
#1661=EDGE_LOOP('',(#6347));
#1662=EDGE_LOOP('',(#6348,#6349,#6350,#6351));
#1663=EDGE_LOOP('',(#6352));
#1664=EDGE_LOOP('',(#6353));
#1665=EDGE_LOOP('',(#6354,#6355,#6356,#6357));
#1666=EDGE_LOOP('',(#6358));
#1667=EDGE_LOOP('',(#6359));
#1668=EDGE_LOOP('',(#6360,#6361,#6362,#6363));
#1669=EDGE_LOOP('',(#6364,#6365,#6366,#6367));
#1670=EDGE_LOOP('',(#6368,#6369,#6370,#6371));
#1671=EDGE_LOOP('',(#6372,#6373,#6374,#6375));
#1672=EDGE_LOOP('',(#6376,#6377,#6378,#6379));
#1673=EDGE_LOOP('',(#6380,#6381,#6382,#6383));
#1674=EDGE_LOOP('',(#6384,#6385,#6386,#6387));
#1675=EDGE_LOOP('',(#6388,#6389,#6390,#6391));
#1676=EDGE_LOOP('',(#6392,#6393,#6394,#6395));
#1677=EDGE_LOOP('',(#6396));
#1678=EDGE_LOOP('',(#6397));
#1679=EDGE_LOOP('',(#6398));
#1680=EDGE_LOOP('',(#6399));
#1681=EDGE_LOOP('',(#6400,#6401,#6402,#6403));
#1682=EDGE_LOOP('',(#6404,#6405,#6406,#6407));
#1683=EDGE_LOOP('',(#6408,#6409,#6410,#6411));
#1684=EDGE_LOOP('',(#6412,#6413,#6414,#6415));
#1685=EDGE_LOOP('',(#6416,#6417,#6418,#6419));
#1686=EDGE_LOOP('',(#6420,#6421,#6422,#6423));
#1687=EDGE_LOOP('',(#6424));
#1688=EDGE_LOOP('',(#6425));
#1689=EDGE_LOOP('',(#6426));
#1690=EDGE_LOOP('',(#6427));
#1691=EDGE_LOOP('',(#6428,#6429,#6430,#6431));
#1692=EDGE_LOOP('',(#6432,#6433,#6434,#6435,#6436,#6437,#6438,#6439,#6440,
#6441,#6442,#6443));
#1693=EDGE_LOOP('',(#6444,#6445,#6446,#6447,#6448,#6449,#6450,#6451,#6452,
#6453,#6454,#6455));
#1694=EDGE_LOOP('',(#6456,#6457,#6458,#6459));
#1695=EDGE_LOOP('',(#6460,#6461,#6462,#6463));
#1696=EDGE_LOOP('',(#6464,#6465,#6466,#6467));
#1697=EDGE_LOOP('',(#6468));
#1698=EDGE_LOOP('',(#6469,#6470,#6471,#6472,#6473,#6474,#6475,#6476,#6477,
#6478));
#1699=EDGE_LOOP('',(#6479,#6480,#6481,#6482));
#1700=EDGE_LOOP('',(#6483,#6484,#6485,#6486));
#1701=EDGE_LOOP('',(#6487,#6488,#6489,#6490,#6491,#6492,#6493,#6494,#6495,
#6496));
#1702=EDGE_LOOP('',(#6497,#6498,#6499,#6500));
#1703=EDGE_LOOP('',(#6501,#6502,#6503,#6504,#6505,#6506));
#1704=EDGE_LOOP('',(#6507,#6508,#6509,#6510,#6511,#6512,#6513,#6514));
#1705=EDGE_LOOP('',(#6515,#6516,#6517,#6518,#6519));
#1706=EDGE_LOOP('',(#6520,#6521,#6522,#6523));
#1707=EDGE_LOOP('',(#6524,#6525,#6526,#6527,#6528,#6529));
#1708=EDGE_LOOP('',(#6530,#6531,#6532,#6533));
#1709=EDGE_LOOP('',(#6534,#6535,#6536,#6537));
#1710=EDGE_LOOP('',(#6538,#6539,#6540,#6541));
#1711=EDGE_LOOP('',(#6542));
#1712=EDGE_LOOP('',(#6543));
#1713=EDGE_LOOP('',(#6544,#6545,#6546,#6547));
#1714=EDGE_LOOP('',(#6548));
#1715=EDGE_LOOP('',(#6549));
#1716=EDGE_LOOP('',(#6550,#6551,#6552,#6553));
#1717=EDGE_LOOP('',(#6554,#6555,#6556,#6557));
#1718=EDGE_LOOP('',(#6558,#6559,#6560,#6561));
#1719=EDGE_LOOP('',(#6562,#6563,#6564,#6565));
#1720=EDGE_LOOP('',(#6566,#6567,#6568,#6569));
#1721=EDGE_LOOP('',(#6570,#6571,#6572,#6573));
#1722=EDGE_LOOP('',(#6574,#6575,#6576,#6577,#6578,#6579));
#1723=EDGE_LOOP('',(#6580,#6581,#6582,#6583,#6584,#6585));
#1724=EDGE_LOOP('',(#6586));
#1725=EDGE_LOOP('',(#6587));
#1726=EDGE_LOOP('',(#6588,#6589,#6590,#6591));
#1727=EDGE_LOOP('',(#6592));
#1728=EDGE_LOOP('',(#6593));
#1729=EDGE_LOOP('',(#6594,#6595,#6596,#6597));
#1730=EDGE_LOOP('',(#6598,#6599,#6600,#6601));
#1731=EDGE_LOOP('',(#6602,#6603,#6604,#6605));
#1732=EDGE_LOOP('',(#6606));
#1733=EDGE_LOOP('',(#6607));
#1734=EDGE_LOOP('',(#6608,#6609,#6610,#6611));
#1735=EDGE_LOOP('',(#6612,#6613,#6614,#6615));
#1736=EDGE_LOOP('',(#6616,#6617,#6618,#6619));
#1737=EDGE_LOOP('',(#6620,#6621,#6622,#6623));
#1738=EDGE_LOOP('',(#6624,#6625,#6626,#6627));
#1739=EDGE_LOOP('',(#6628,#6629,#6630,#6631));
#1740=EDGE_LOOP('',(#6632,#6633,#6634,#6635));
#1741=EDGE_LOOP('',(#6636,#6637,#6638,#6639));
#1742=EDGE_LOOP('',(#6640,#6641,#6642,#6643));
#1743=EDGE_LOOP('',(#6644,#6645,#6646,#6647));
#1744=EDGE_LOOP('',(#6648,#6649,#6650,#6651));
#1745=EDGE_LOOP('',(#6652,#6653,#6654,#6655,#6656,#6657,#6658,#6659));
#1746=EDGE_LOOP('',(#6660));
#1747=EDGE_LOOP('',(#6661));
#1748=EDGE_LOOP('',(#6662));
#1749=EDGE_LOOP('',(#6663));
#1750=EDGE_LOOP('',(#6664));
#1751=EDGE_LOOP('',(#6665));
#1752=EDGE_LOOP('',(#6666,#6667,#6668,#6669));
#1753=EDGE_LOOP('',(#6670,#6671,#6672,#6673));
#1754=EDGE_LOOP('',(#6674,#6675,#6676,#6677));
#1755=EDGE_LOOP('',(#6678,#6679,#6680,#6681));
#1756=EDGE_LOOP('',(#6682,#6683,#6684,#6685));
#1757=EDGE_LOOP('',(#6686,#6687,#6688,#6689,#6690,#6691,#6692,#6693));
#1758=EDGE_LOOP('',(#6694));
#1759=EDGE_LOOP('',(#6695));
#1760=EDGE_LOOP('',(#6696));
#1761=EDGE_LOOP('',(#6697));
#1762=EDGE_LOOP('',(#6698));
#1763=EDGE_LOOP('',(#6699));
#1764=EDGE_LOOP('',(#6700,#6701,#6702,#6703));
#1765=EDGE_LOOP('',(#6704));
#1766=EDGE_LOOP('',(#6705,#6706,#6707,#6708));
#1767=EDGE_LOOP('',(#6709));
#1768=EDGE_LOOP('',(#6710,#6711,#6712,#6713,#6714));
#1769=EDGE_LOOP('',(#6715));
#1770=EDGE_LOOP('',(#6716));
#1771=EDGE_LOOP('',(#6717,#6718));
#1772=EDGE_LOOP('',(#6719,#6720,#6721));
#1773=EDGE_LOOP('',(#6722,#6723,#6724,#6725,#6726));
#1774=EDGE_LOOP('',(#6727));
#1775=EDGE_LOOP('',(#6728));
#1776=EDGE_LOOP('',(#6729,#6730));
#1777=EDGE_LOOP('',(#6731,#6732,#6733));
#1778=EDGE_LOOP('',(#6734,#6735,#6736,#6737,#6738,#6739,#6740,#6741));
#1779=EDGE_LOOP('',(#6742,#6743));
#1780=EDGE_LOOP('',(#6744,#6745,#6746,#6747,#6748,#6749,#6750,#6751));
#1781=EDGE_LOOP('',(#6752,#6753));
#1782=EDGE_LOOP('',(#6754,#6755,#6756,#6757,#6758,#6759,#6760,#6761));
#1783=EDGE_LOOP('',(#6762,#6763));
#1784=EDGE_LOOP('',(#6764,#6765,#6766,#6767,#6768,#6769,#6770,#6771));
#1785=EDGE_LOOP('',(#6772,#6773));
#1786=EDGE_LOOP('',(#6774,#6775,#6776,#6777,#6778,#6779,#6780,#6781));
#1787=EDGE_LOOP('',(#6782,#6783,#6784,#6785,#6786,#6787,#6788,#6789,#6790,
#6791,#6792,#6793));
#1788=EDGE_LOOP('',(#6794,#6795,#6796,#6797,#6798,#6799,#6800,#6801,#6802,
#6803,#6804,#6805));
#1789=EDGE_LOOP('',(#6806,#6807,#6808,#6809,#6810,#6811,#6812,#6813,#6814,
#6815,#6816,#6817));
#1790=EDGE_LOOP('',(#6818,#6819,#6820,#6821,#6822,#6823,#6824,#6825,#6826,
#6827));
#1791=EDGE_LOOP('',(#6828,#6829,#6830,#6831));
#1792=EDGE_LOOP('',(#6832,#6833,#6834,#6835));
#1793=EDGE_LOOP('',(#6836));
#1794=EDGE_LOOP('',(#6837));
#1795=EDGE_LOOP('',(#6838));
#1796=EDGE_LOOP('',(#6839));
#1797=EDGE_LOOP('',(#6840,#6841,#6842,#6843));
#1798=EDGE_LOOP('',(#6844,#6845,#6846,#6847,#6848,#6849,#6850,#6851,#6852,
#6853));
#1799=EDGE_LOOP('',(#6854,#6855,#6856,#6857));
#1800=EDGE_LOOP('',(#6858,#6859,#6860,#6861));
#1801=EDGE_LOOP('',(#6862,#6863,#6864,#6865));
#1802=EDGE_LOOP('',(#6866,#6867,#6868,#6869));
#1803=EDGE_LOOP('',(#6870,#6871,#6872,#6873));
#1804=EDGE_LOOP('',(#6874,#6875,#6876,#6877,#6878,#6879,#6880,#6881,#6882,
#6883,#6884,#6885));
#1805=EDGE_LOOP('',(#6886,#6887,#6888,#6889));
#1806=EDGE_LOOP('',(#6890,#6891,#6892,#6893));
#1807=EDGE_LOOP('',(#6894,#6895,#6896,#6897));
#1808=EDGE_LOOP('',(#6898,#6899,#6900,#6901));
#1809=EDGE_LOOP('',(#6902,#6903,#6904,#6905));
#1810=EDGE_LOOP('',(#6906,#6907,#6908,#6909));
#1811=EDGE_LOOP('',(#6910,#6911,#6912,#6913));
#1812=EDGE_LOOP('',(#6914,#6915,#6916,#6917));
#1813=EDGE_LOOP('',(#6918,#6919,#6920,#6921,#6922,#6923,#6924,#6925));
#1814=EDGE_LOOP('',(#6926,#6927,#6928,#6929,#6930,#6931,#6932,#6933));
#1815=EDGE_LOOP('',(#6934,#6935,#6936,#6937));
#1816=EDGE_LOOP('',(#6938,#6939,#6940,#6941));
#1817=EDGE_LOOP('',(#6942,#6943,#6944,#6945));
#1818=EDGE_LOOP('',(#6946,#6947,#6948,#6949));
#1819=EDGE_LOOP('',(#6950,#6951,#6952,#6953));
#1820=EDGE_LOOP('',(#6954,#6955,#6956,#6957));
#1821=EDGE_LOOP('',(#6958,#6959,#6960,#6961));
#1822=EDGE_LOOP('',(#6962,#6963,#6964,#6965));
#1823=EDGE_LOOP('',(#6966,#6967,#6968,#6969,#6970,#6971,#6972,#6973));
#1824=EDGE_LOOP('',(#6974,#6975,#6976,#6977,#6978,#6979,#6980,#6981));
#1825=EDGE_LOOP('',(#6982,#6983,#6984,#6985));
#1826=EDGE_LOOP('',(#6986,#6987,#6988,#6989));
#1827=EDGE_LOOP('',(#6990,#6991,#6992,#6993));
#1828=EDGE_LOOP('',(#6994,#6995,#6996,#6997));
#1829=EDGE_LOOP('',(#6998,#6999,#7000,#7001));
#1830=EDGE_LOOP('',(#7002,#7003,#7004,#7005));
#1831=EDGE_LOOP('',(#7006,#7007,#7008,#7009,#7010,#7011));
#1832=EDGE_LOOP('',(#7012,#7013,#7014,#7015,#7016,#7017));
#1833=EDGE_LOOP('',(#7018));
#1834=EDGE_LOOP('',(#7019));
#1835=EDGE_LOOP('',(#7020,#7021,#7022,#7023));
#1836=EDGE_LOOP('',(#7024,#7025,#7026,#7027));
#1837=EDGE_LOOP('',(#7028,#7029,#7030,#7031));
#1838=EDGE_LOOP('',(#7032));
#1839=EDGE_LOOP('',(#7033));
#1840=EDGE_LOOP('',(#7034,#7035,#7036,#7037));
#1841=EDGE_LOOP('',(#7038,#7039,#7040,#7041));
#1842=EDGE_LOOP('',(#7042));
#1843=EDGE_LOOP('',(#7043,#7044,#7045,#7046));
#1844=EDGE_LOOP('',(#7047,#7048,#7049,#7050));
#1845=EDGE_LOOP('',(#7051,#7052,#7053,#7054));
#1846=EDGE_LOOP('',(#7055));
#1847=EDGE_LOOP('',(#7056));
#1848=EDGE_LOOP('',(#7057,#7058,#7059,#7060));
#1849=EDGE_LOOP('',(#7061,#7062,#7063,#7064));
#1850=EDGE_LOOP('',(#7065,#7066,#7067,#7068));
#1851=EDGE_LOOP('',(#7069));
#1852=EDGE_LOOP('',(#7070,#7071,#7072,#7073));
#1853=EDGE_LOOP('',(#7074,#7075,#7076,#7077));
#1854=EDGE_LOOP('',(#7078,#7079,#7080,#7081));
#1855=EDGE_LOOP('',(#7082,#7083,#7084,#7085));
#1856=EDGE_LOOP('',(#7086,#7087,#7088,#7089));
#1857=EDGE_LOOP('',(#7090,#7091,#7092,#7093));
#1858=EDGE_LOOP('',(#7094,#7095,#7096,#7097,#7098,#7099));
#1859=EDGE_LOOP('',(#7100,#7101,#7102,#7103,#7104,#7105));
#1860=LINE('',#10906,#2637);
#1861=LINE('',#10912,#2638);
#1862=LINE('',#10918,#2639);
#1863=LINE('',#10924,#2640);
#1864=LINE('',#10929,#2641);
#1865=LINE('',#10931,#2642);
#1866=LINE('',#10933,#2643);
#1867=LINE('',#10934,#2644);
#1868=LINE('',#10937,#2645);
#1869=LINE('',#10939,#2646);
#1870=LINE('',#10940,#2647);
#1871=LINE('',#10943,#2648);
#1872=LINE('',#10945,#2649);
#1873=LINE('',#10946,#2650);
#1874=LINE('',#10948,#2651);
#1875=LINE('',#10949,#2652);
#1876=LINE('',#10957,#2653);
#1877=LINE('',#10963,#2654);
#1878=LINE('',#10969,#2655);
#1879=LINE('',#10975,#2656);
#1880=LINE('',#10980,#2657);
#1881=LINE('',#10982,#2658);
#1882=LINE('',#10984,#2659);
#1883=LINE('',#10985,#2660);
#1884=LINE('',#10988,#2661);
#1885=LINE('',#10990,#2662);
#1886=LINE('',#10991,#2663);
#1887=LINE('',#10994,#2664);
#1888=LINE('',#10996,#2665);
#1889=LINE('',#10997,#2666);
#1890=LINE('',#10999,#2667);
#1891=LINE('',#11000,#2668);
#1892=LINE('',#11004,#2669);
#1893=LINE('',#11006,#2670);
#1894=LINE('',#11008,#2671);
#1895=LINE('',#11009,#2672);
#1896=LINE('',#11012,#2673);
#1897=LINE('',#11014,#2674);
#1898=LINE('',#11015,#2675);
#1899=LINE('',#11018,#2676);
#1900=LINE('',#11020,#2677);
#1901=LINE('',#11021,#2678);
#1902=LINE('',#11023,#2679);
#1903=LINE('',#11024,#2680);
#1904=LINE('',#11031,#2681);
#1905=LINE('',#11033,#2682);
#1906=LINE('',#11035,#2683);
#1907=LINE('',#11036,#2684);
#1908=LINE('',#11039,#2685);
#1909=LINE('',#11041,#2686);
#1910=LINE('',#11042,#2687);
#1911=LINE('',#11045,#2688);
#1912=LINE('',#11047,#2689);
#1913=LINE('',#11048,#2690);
#1914=LINE('',#11050,#2691);
#1915=LINE('',#11051,#2692);
#1916=LINE('',#11058,#2693);
#1917=LINE('',#11060,#2694);
#1918=LINE('',#11062,#2695);
#1919=LINE('',#11063,#2696);
#1920=LINE('',#11066,#2697);
#1921=LINE('',#11068,#2698);
#1922=LINE('',#11069,#2699);
#1923=LINE('',#11072,#2700);
#1924=LINE('',#11074,#2701);
#1925=LINE('',#11075,#2702);
#1926=LINE('',#11077,#2703);
#1927=LINE('',#11078,#2704);
#1928=LINE('',#11085,#2705);
#1929=LINE('',#11087,#2706);
#1930=LINE('',#11089,#2707);
#1931=LINE('',#11090,#2708);
#1932=LINE('',#11093,#2709);
#1933=LINE('',#11095,#2710);
#1934=LINE('',#11096,#2711);
#1935=LINE('',#11099,#2712);
#1936=LINE('',#11101,#2713);
#1937=LINE('',#11102,#2714);
#1938=LINE('',#11104,#2715);
#1939=LINE('',#11105,#2716);
#1940=LINE('',#11113,#2717);
#1941=LINE('',#11119,#2718);
#1942=LINE('',#11124,#2719);
#1943=LINE('',#11126,#2720);
#1944=LINE('',#11128,#2721);
#1945=LINE('',#11129,#2722);
#1946=LINE('',#11132,#2723);
#1947=LINE('',#11134,#2724);
#1948=LINE('',#11135,#2725);
#1949=LINE('',#11138,#2726);
#1950=LINE('',#11140,#2727);
#1951=LINE('',#11141,#2728);
#1952=LINE('',#11143,#2729);
#1953=LINE('',#11144,#2730);
#1954=LINE('',#11152,#2731);
#1955=LINE('',#11158,#2732);
#1956=LINE('',#11163,#2733);
#1957=LINE('',#11165,#2734);
#1958=LINE('',#11167,#2735);
#1959=LINE('',#11168,#2736);
#1960=LINE('',#11171,#2737);
#1961=LINE('',#11173,#2738);
#1962=LINE('',#11174,#2739);
#1963=LINE('',#11177,#2740);
#1964=LINE('',#11179,#2741);
#1965=LINE('',#11180,#2742);
#1966=LINE('',#11182,#2743);
#1967=LINE('',#11183,#2744);
#1968=LINE('',#11191,#2745);
#1969=LINE('',#11198,#2746);
#1970=LINE('',#11206,#2747);
#1971=LINE('',#11210,#2748);
#1972=LINE('',#11212,#2749);
#1973=LINE('',#11214,#2750);
#1974=LINE('',#11215,#2751);
#1975=LINE('',#11218,#2752);
#1976=LINE('',#11220,#2753);
#1977=LINE('',#11221,#2754);
#1978=LINE('',#11224,#2755);
#1979=LINE('',#11226,#2756);
#1980=LINE('',#11227,#2757);
#1981=LINE('',#11229,#2758);
#1982=LINE('',#11230,#2759);
#1983=LINE('',#11238,#2760);
#1984=LINE('',#11245,#2761);
#1985=LINE('',#11252,#2762);
#1986=LINE('',#11257,#2763);
#1987=LINE('',#11259,#2764);
#1988=LINE('',#11261,#2765);
#1989=LINE('',#11262,#2766);
#1990=LINE('',#11265,#2767);
#1991=LINE('',#11267,#2768);
#1992=LINE('',#11268,#2769);
#1993=LINE('',#11271,#2770);
#1994=LINE('',#11273,#2771);
#1995=LINE('',#11274,#2772);
#1996=LINE('',#11276,#2773);
#1997=LINE('',#11277,#2774);
#1998=LINE('',#11285,#2775);
#1999=LINE('',#11292,#2776);
#2000=LINE('',#11300,#2777);
#2001=LINE('',#11304,#2778);
#2002=LINE('',#11306,#2779);
#2003=LINE('',#11308,#2780);
#2004=LINE('',#11309,#2781);
#2005=LINE('',#11312,#2782);
#2006=LINE('',#11314,#2783);
#2007=LINE('',#11315,#2784);
#2008=LINE('',#11318,#2785);
#2009=LINE('',#11320,#2786);
#2010=LINE('',#11321,#2787);
#2011=LINE('',#11323,#2788);
#2012=LINE('',#11324,#2789);
#2013=LINE('',#11332,#2790);
#2014=LINE('',#11339,#2791);
#2015=LINE('',#11346,#2792);
#2016=LINE('',#11351,#2793);
#2017=LINE('',#11353,#2794);
#2018=LINE('',#11355,#2795);
#2019=LINE('',#11356,#2796);
#2020=LINE('',#11359,#2797);
#2021=LINE('',#11361,#2798);
#2022=LINE('',#11362,#2799);
#2023=LINE('',#11365,#2800);
#2024=LINE('',#11367,#2801);
#2025=LINE('',#11368,#2802);
#2026=LINE('',#11370,#2803);
#2027=LINE('',#11371,#2804);
#2028=LINE('',#11378,#2805);
#2029=LINE('',#11380,#2806);
#2030=LINE('',#11382,#2807);
#2031=LINE('',#11383,#2808);
#2032=LINE('',#11386,#2809);
#2033=LINE('',#11388,#2810);
#2034=LINE('',#11389,#2811);
#2035=LINE('',#11392,#2812);
#2036=LINE('',#11394,#2813);
#2037=LINE('',#11395,#2814);
#2038=LINE('',#11397,#2815);
#2039=LINE('',#11398,#2816);
#2040=LINE('',#11402,#2817);
#2041=LINE('',#11404,#2818);
#2042=LINE('',#11406,#2819);
#2043=LINE('',#11407,#2820);
#2044=LINE('',#11410,#2821);
#2045=LINE('',#11412,#2822);
#2046=LINE('',#11413,#2823);
#2047=LINE('',#11416,#2824);
#2048=LINE('',#11418,#2825);
#2049=LINE('',#11419,#2826);
#2050=LINE('',#11421,#2827);
#2051=LINE('',#11422,#2828);
#2052=LINE('',#11429,#2829);
#2053=LINE('',#11431,#2830);
#2054=LINE('',#11433,#2831);
#2055=LINE('',#11434,#2832);
#2056=LINE('',#11437,#2833);
#2057=LINE('',#11439,#2834);
#2058=LINE('',#11440,#2835);
#2059=LINE('',#11443,#2836);
#2060=LINE('',#11445,#2837);
#2061=LINE('',#11446,#2838);
#2062=LINE('',#11448,#2839);
#2063=LINE('',#11449,#2840);
#2064=LINE('',#11453,#2841);
#2065=LINE('',#11455,#2842);
#2066=LINE('',#11457,#2843);
#2067=LINE('',#11458,#2844);
#2068=LINE('',#11461,#2845);
#2069=LINE('',#11463,#2846);
#2070=LINE('',#11464,#2847);
#2071=LINE('',#11467,#2848);
#2072=LINE('',#11469,#2849);
#2073=LINE('',#11470,#2850);
#2074=LINE('',#11472,#2851);
#2075=LINE('',#11473,#2852);
#2076=LINE('',#11481,#2853);
#2077=LINE('',#11487,#2854);
#2078=LINE('',#11493,#2855);
#2079=LINE('',#11499,#2856);
#2080=LINE('',#11505,#2857);
#2081=LINE('',#11511,#2858);
#2082=LINE('',#11517,#2859);
#2083=LINE('',#11523,#2860);
#2084=LINE('',#11528,#2861);
#2085=LINE('',#11530,#2862);
#2086=LINE('',#11532,#2863);
#2087=LINE('',#11533,#2864);
#2088=LINE('',#11536,#2865);
#2089=LINE('',#11538,#2866);
#2090=LINE('',#11539,#2867);
#2091=LINE('',#11542,#2868);
#2092=LINE('',#11544,#2869);
#2093=LINE('',#11545,#2870);
#2094=LINE('',#11547,#2871);
#2095=LINE('',#11548,#2872);
#2096=LINE('',#11556,#2873);
#2097=LINE('',#11562,#2874);
#2098=LINE('',#11567,#2875);
#2099=LINE('',#11569,#2876);
#2100=LINE('',#11571,#2877);
#2101=LINE('',#11572,#2878);
#2102=LINE('',#11575,#2879);
#2103=LINE('',#11577,#2880);
#2104=LINE('',#11578,#2881);
#2105=LINE('',#11581,#2882);
#2106=LINE('',#11583,#2883);
#2107=LINE('',#11584,#2884);
#2108=LINE('',#11587,#2885);
#2109=LINE('',#11589,#2886);
#2110=LINE('',#11590,#2887);
#2111=LINE('',#11593,#2888);
#2112=LINE('',#11595,#2889);
#2113=LINE('',#11596,#2890);
#2114=LINE('',#11598,#2891);
#2115=LINE('',#11599,#2892);
#2116=LINE('',#11607,#2893);
#2117=LINE('',#11614,#2894);
#2118=LINE('',#11619,#2895);
#2119=LINE('',#11621,#2896);
#2120=LINE('',#11623,#2897);
#2121=LINE('',#11624,#2898);
#2122=LINE('',#11627,#2899);
#2123=LINE('',#11629,#2900);
#2124=LINE('',#11630,#2901);
#2125=LINE('',#11633,#2902);
#2126=LINE('',#11634,#2903);
#2127=LINE('',#11637,#2904);
#2128=LINE('',#11639,#2905);
#2129=LINE('',#11641,#2906);
#2130=LINE('',#11642,#2907);
#2131=LINE('',#11645,#2908);
#2132=LINE('',#11647,#2909);
#2133=LINE('',#11648,#2910);
#2134=LINE('',#11651,#2911);
#2135=LINE('',#11652,#2912);
#2136=LINE('',#11655,#2913);
#2137=LINE('',#11656,#2914);
#2138=LINE('',#11658,#2915);
#2139=LINE('',#11665,#2916);
#2140=LINE('',#11672,#2917);
#2141=LINE('',#11677,#2918);
#2142=LINE('',#11679,#2919);
#2143=LINE('',#11681,#2920);
#2144=LINE('',#11682,#2921);
#2145=LINE('',#11685,#2922);
#2146=LINE('',#11687,#2923);
#2147=LINE('',#11688,#2924);
#2148=LINE('',#11691,#2925);
#2149=LINE('',#11692,#2926);
#2150=LINE('',#11695,#2927);
#2151=LINE('',#11697,#2928);
#2152=LINE('',#11699,#2929);
#2153=LINE('',#11700,#2930);
#2154=LINE('',#11703,#2931);
#2155=LINE('',#11705,#2932);
#2156=LINE('',#11706,#2933);
#2157=LINE('',#11709,#2934);
#2158=LINE('',#11710,#2935);
#2159=LINE('',#11713,#2936);
#2160=LINE('',#11714,#2937);
#2161=LINE('',#11716,#2938);
#2162=LINE('',#11723,#2939);
#2163=LINE('',#11728,#2940);
#2164=LINE('',#11730,#2941);
#2165=LINE('',#11732,#2942);
#2166=LINE('',#11733,#2943);
#2167=LINE('',#11736,#2944);
#2168=LINE('',#11738,#2945);
#2169=LINE('',#11739,#2946);
#2170=LINE('',#11742,#2947);
#2171=LINE('',#11744,#2948);
#2172=LINE('',#11745,#2949);
#2173=LINE('',#11747,#2950);
#2174=LINE('',#11748,#2951);
#2175=LINE('',#11756,#2952);
#2176=LINE('',#11761,#2953);
#2177=LINE('',#11763,#2954);
#2178=LINE('',#11765,#2955);
#2179=LINE('',#11766,#2956);
#2180=LINE('',#11769,#2957);
#2181=LINE('',#11771,#2958);
#2182=LINE('',#11772,#2959);
#2183=LINE('',#11775,#2960);
#2184=LINE('',#11777,#2961);
#2185=LINE('',#11778,#2962);
#2186=LINE('',#11780,#2963);
#2187=LINE('',#11781,#2964);
#2188=LINE('',#11788,#2965);
#2189=LINE('',#11790,#2966);
#2190=LINE('',#11792,#2967);
#2191=LINE('',#11793,#2968);
#2192=LINE('',#11796,#2969);
#2193=LINE('',#11798,#2970);
#2194=LINE('',#11799,#2971);
#2195=LINE('',#11802,#2972);
#2196=LINE('',#11804,#2973);
#2197=LINE('',#11805,#2974);
#2198=LINE('',#11808,#2975);
#2199=LINE('',#11810,#2976);
#2200=LINE('',#11811,#2977);
#2201=LINE('',#11814,#2978);
#2202=LINE('',#11816,#2979);
#2203=LINE('',#11817,#2980);
#2204=LINE('',#11820,#2981);
#2205=LINE('',#11822,#2982);
#2206=LINE('',#11823,#2983);
#2207=LINE('',#11826,#2984);
#2208=LINE('',#11828,#2985);
#2209=LINE('',#11829,#2986);
#2210=LINE('',#11832,#2987);
#2211=LINE('',#11834,#2988);
#2212=LINE('',#11835,#2989);
#2213=LINE('',#11838,#2990);
#2214=LINE('',#11840,#2991);
#2215=LINE('',#11841,#2992);
#2216=LINE('',#11845,#2993);
#2217=LINE('',#11847,#2994);
#2218=LINE('',#11849,#2995);
#2219=LINE('',#11850,#2996);
#2220=LINE('',#11853,#2997);
#2221=LINE('',#11855,#2998);
#2222=LINE('',#11856,#2999);
#2223=LINE('',#11859,#3000);
#2224=LINE('',#11861,#3001);
#2225=LINE('',#11862,#3002);
#2226=LINE('',#11865,#3003);
#2227=LINE('',#11867,#3004);
#2228=LINE('',#11868,#3005);
#2229=LINE('',#11871,#3006);
#2230=LINE('',#11873,#3007);
#2231=LINE('',#11874,#3008);
#2232=LINE('',#11877,#3009);
#2233=LINE('',#11879,#3010);
#2234=LINE('',#11880,#3011);
#2235=LINE('',#11883,#3012);
#2236=LINE('',#11885,#3013);
#2237=LINE('',#11886,#3014);
#2238=LINE('',#11889,#3015);
#2239=LINE('',#11891,#3016);
#2240=LINE('',#11892,#3017);
#2241=LINE('',#11895,#3018);
#2242=LINE('',#11897,#3019);
#2243=LINE('',#11898,#3020);
#2244=LINE('',#11902,#3021);
#2245=LINE('',#11904,#3022);
#2246=LINE('',#11906,#3023);
#2247=LINE('',#11907,#3024);
#2248=LINE('',#11910,#3025);
#2249=LINE('',#11912,#3026);
#2250=LINE('',#11913,#3027);
#2251=LINE('',#11916,#3028);
#2252=LINE('',#11918,#3029);
#2253=LINE('',#11919,#3030);
#2254=LINE('',#11922,#3031);
#2255=LINE('',#11924,#3032);
#2256=LINE('',#11925,#3033);
#2257=LINE('',#11928,#3034);
#2258=LINE('',#11930,#3035);
#2259=LINE('',#11931,#3036);
#2260=LINE('',#11934,#3037);
#2261=LINE('',#11936,#3038);
#2262=LINE('',#11937,#3039);
#2263=LINE('',#11940,#3040);
#2264=LINE('',#11942,#3041);
#2265=LINE('',#11943,#3042);
#2266=LINE('',#11946,#3043);
#2267=LINE('',#11948,#3044);
#2268=LINE('',#11949,#3045);
#2269=LINE('',#11952,#3046);
#2270=LINE('',#11954,#3047);
#2271=LINE('',#11955,#3048);
#2272=LINE('',#11959,#3049);
#2273=LINE('',#11961,#3050);
#2274=LINE('',#11963,#3051);
#2275=LINE('',#11964,#3052);
#2276=LINE('',#11967,#3053);
#2277=LINE('',#11969,#3054);
#2278=LINE('',#11970,#3055);
#2279=LINE('',#11973,#3056);
#2280=LINE('',#11975,#3057);
#2281=LINE('',#11976,#3058);
#2282=LINE('',#11979,#3059);
#2283=LINE('',#11981,#3060);
#2284=LINE('',#11982,#3061);
#2285=LINE('',#11985,#3062);
#2286=LINE('',#11987,#3063);
#2287=LINE('',#11988,#3064);
#2288=LINE('',#11991,#3065);
#2289=LINE('',#11993,#3066);
#2290=LINE('',#11994,#3067);
#2291=LINE('',#11997,#3068);
#2292=LINE('',#11999,#3069);
#2293=LINE('',#12000,#3070);
#2294=LINE('',#12003,#3071);
#2295=LINE('',#12005,#3072);
#2296=LINE('',#12006,#3073);
#2297=LINE('',#12009,#3074);
#2298=LINE('',#12011,#3075);
#2299=LINE('',#12012,#3076);
#2300=LINE('',#12017,#3077);
#2301=LINE('',#12021,#3078);
#2302=LINE('',#12023,#3079);
#2303=LINE('',#12024,#3080);
#2304=LINE('',#12027,#3081);
#2305=LINE('',#12029,#3082);
#2306=LINE('',#12030,#3083);
#2307=LINE('',#12032,#3084);
#2308=LINE('',#12033,#3085);
#2309=LINE('',#12036,#3086);
#2310=LINE('',#12038,#3087);
#2311=LINE('',#12039,#3088);
#2312=LINE('',#12041,#3089);
#2313=LINE('',#12042,#3090);
#2314=LINE('',#12045,#3091);
#2315=LINE('',#12047,#3092);
#2316=LINE('',#12048,#3093);
#2317=LINE('',#12050,#3094);
#2318=LINE('',#12051,#3095);
#2319=LINE('',#12053,#3096);
#2320=LINE('',#12054,#3097);
#2321=LINE('',#12064,#3098);
#2322=LINE('',#12068,#3099);
#2323=LINE('',#12072,#3100);
#2324=LINE('',#12079,#3101);
#2325=LINE('',#12083,#3102);
#2326=LINE('',#12087,#3103);
#2327=LINE('',#12092,#3104);
#2328=LINE('',#12094,#3105);
#2329=LINE('',#12096,#3106);
#2330=LINE('',#12097,#3107);
#2331=LINE('',#12100,#3108);
#2332=LINE('',#12102,#3109);
#2333=LINE('',#12103,#3110);
#2334=LINE('',#12106,#3111);
#2335=LINE('',#12108,#3112);
#2336=LINE('',#12109,#3113);
#2337=LINE('',#12112,#3114);
#2338=LINE('',#12114,#3115);
#2339=LINE('',#12115,#3116);
#2340=LINE('',#12118,#3117);
#2341=LINE('',#12120,#3118);
#2342=LINE('',#12121,#3119);
#2343=LINE('',#12123,#3120);
#2344=LINE('',#12124,#3121);
#2345=LINE('',#12132,#3122);
#2346=LINE('',#12141,#3123);
#2347=LINE('',#12150,#3124);
#2348=LINE('',#12159,#3125);
#2349=LINE('',#12167,#3126);
#2350=LINE('',#12171,#3127);
#2351=LINE('',#12175,#3128);
#2352=LINE('',#12179,#3129);
#2353=LINE('',#12183,#3130);
#2354=LINE('',#12185,#3131);
#2355=LINE('',#12187,#3132);
#2356=LINE('',#12188,#3133);
#2357=LINE('',#12191,#3134);
#2358=LINE('',#12193,#3135);
#2359=LINE('',#12194,#3136);
#2360=LINE('',#12197,#3137);
#2361=LINE('',#12199,#3138);
#2362=LINE('',#12200,#3139);
#2363=LINE('',#12203,#3140);
#2364=LINE('',#12205,#3141);
#2365=LINE('',#12206,#3142);
#2366=LINE('',#12209,#3143);
#2367=LINE('',#12211,#3144);
#2368=LINE('',#12212,#3145);
#2369=LINE('',#12215,#3146);
#2370=LINE('',#12217,#3147);
#2371=LINE('',#12218,#3148);
#2372=LINE('',#12221,#3149);
#2373=LINE('',#12223,#3150);
#2374=LINE('',#12224,#3151);
#2375=LINE('',#12227,#3152);
#2376=LINE('',#12229,#3153);
#2377=LINE('',#12230,#3154);
#2378=LINE('',#12233,#3155);
#2379=LINE('',#12235,#3156);
#2380=LINE('',#12236,#3157);
#2381=LINE('',#12239,#3158);
#2382=LINE('',#12241,#3159);
#2383=LINE('',#12242,#3160);
#2384=LINE('',#12245,#3161);
#2385=LINE('',#12247,#3162);
#2386=LINE('',#12248,#3163);
#2387=LINE('',#12250,#3164);
#2388=LINE('',#12251,#3165);
#2389=LINE('',#12258,#3166);
#2390=LINE('',#12260,#3167);
#2391=LINE('',#12262,#3168);
#2392=LINE('',#12263,#3169);
#2393=LINE('',#12266,#3170);
#2394=LINE('',#12268,#3171);
#2395=LINE('',#12269,#3172);
#2396=LINE('',#12272,#3173);
#2397=LINE('',#12274,#3174);
#2398=LINE('',#12275,#3175);
#2399=LINE('',#12280,#3176);
#2400=LINE('',#12282,#3177);
#2401=LINE('',#12284,#3178);
#2402=LINE('',#12286,#3179);
#2403=LINE('',#12288,#3180);
#2404=LINE('',#12290,#3181);
#2405=LINE('',#12291,#3182);
#2406=LINE('',#12294,#3183);
#2407=LINE('',#12295,#3184);
#2408=LINE('',#12298,#3185);
#2409=LINE('',#12299,#3186);
#2410=LINE('',#12302,#3187);
#2411=LINE('',#12304,#3188);
#2412=LINE('',#12306,#3189);
#2413=LINE('',#12308,#3190);
#2414=LINE('',#12309,#3191);
#2415=LINE('',#12311,#3192);
#2416=LINE('',#12314,#3193);
#2417=LINE('',#12317,#3194);
#2418=LINE('',#12321,#3195);
#2419=LINE('',#12328,#3196);
#2420=LINE('',#12330,#3197);
#2421=LINE('',#12332,#3198);
#2422=LINE('',#12339,#3199);
#2423=LINE('',#12343,#3200);
#2424=LINE('',#12350,#3201);
#2425=LINE('',#12357,#3202);
#2426=LINE('',#12359,#3203);
#2427=LINE('',#12361,#3204);
#2428=LINE('',#12362,#3205);
#2429=LINE('',#12365,#3206);
#2430=LINE('',#12367,#3207);
#2431=LINE('',#12368,#3208);
#2432=LINE('',#12371,#3209);
#2433=LINE('',#12373,#3210);
#2434=LINE('',#12374,#3211);
#2435=LINE('',#12377,#3212);
#2436=LINE('',#12379,#3213);
#2437=LINE('',#12380,#3214);
#2438=LINE('',#12383,#3215);
#2439=LINE('',#12385,#3216);
#2440=LINE('',#12386,#3217);
#2441=LINE('',#12388,#3218);
#2442=LINE('',#12389,#3219);
#2443=LINE('',#12399,#3220);
#2444=LINE('',#12408,#3221);
#2445=LINE('',#12412,#3222);
#2446=LINE('',#12416,#3223);
#2447=LINE('',#12423,#3224);
#2448=LINE('',#12425,#3225);
#2449=LINE('',#12432,#3226);
#2450=LINE('',#12438,#3227);
#2451=LINE('',#12444,#3228);
#2452=LINE('',#12450,#3229);
#2453=LINE('',#12456,#3230);
#2454=LINE('',#12462,#3231);
#2455=LINE('',#12467,#3232);
#2456=LINE('',#12469,#3233);
#2457=LINE('',#12471,#3234);
#2458=LINE('',#12472,#3235);
#2459=LINE('',#12476,#3236);
#2460=LINE('',#12478,#3237);
#2461=LINE('',#12480,#3238);
#2462=LINE('',#12481,#3239);
#2463=LINE('',#12483,#3240);
#2464=LINE('',#12484,#3241);
#2465=LINE('',#12487,#3242);
#2466=LINE('',#12489,#3243);
#2467=LINE('',#12491,#3244);
#2468=LINE('',#12493,#3245);
#2469=LINE('',#12494,#3246);
#2470=LINE('',#12497,#3247);
#2471=LINE('',#12498,#3248);
#2472=LINE('',#12501,#3249);
#2473=LINE('',#12503,#3250);
#2474=LINE('',#12504,#3251);
#2475=LINE('',#12506,#3252);
#2476=LINE('',#12509,#3253);
#2477=LINE('',#12510,#3254);
#2478=LINE('',#12512,#3255);
#2479=LINE('',#12519,#3256);
#2480=LINE('',#12526,#3257);
#2481=LINE('',#12533,#3258);
#2482=LINE('',#12539,#3259);
#2483=LINE('',#12548,#3260);
#2484=LINE('',#12554,#3261);
#2485=LINE('',#12560,#3262);
#2486=LINE('',#12566,#3263);
#2487=LINE('',#12570,#3264);
#2488=LINE('',#12574,#3265);
#2489=LINE('',#12578,#3266);
#2490=LINE('',#12582,#3267);
#2491=LINE('',#12586,#3268);
#2492=LINE('',#12590,#3269);
#2493=LINE('',#12594,#3270);
#2494=LINE('',#12598,#3271);
#2495=LINE('',#12602,#3272);
#2496=LINE('',#12606,#3273);
#2497=LINE('',#12610,#3274);
#2498=LINE('',#12614,#3275);
#2499=LINE('',#12618,#3276);
#2500=LINE('',#12622,#3277);
#2501=LINE('',#12626,#3278);
#2502=LINE('',#12628,#3279);
#2503=LINE('',#12630,#3280);
#2504=LINE('',#12632,#3281);
#2505=LINE('',#12634,#3282);
#2506=LINE('',#12636,#3283);
#2507=LINE('',#12637,#3284);
#2508=LINE('',#12639,#3285);
#2509=LINE('',#12641,#3286);
#2510=LINE('',#12643,#3287);
#2511=LINE('',#12645,#3288);
#2512=LINE('',#12647,#3289);
#2513=LINE('',#12648,#3290);
#2514=LINE('',#12651,#3291);
#2515=LINE('',#12653,#3292);
#2516=LINE('',#12655,#3293);
#2517=LINE('',#12657,#3294);
#2518=LINE('',#12658,#3295);
#2519=LINE('',#12660,#3296);
#2520=LINE('',#12662,#3297);
#2521=LINE('',#12664,#3298);
#2522=LINE('',#12666,#3299);
#2523=LINE('',#12667,#3300);
#2524=LINE('',#12670,#3301);
#2525=LINE('',#12671,#3302);
#2526=LINE('',#12674,#3303);
#2527=LINE('',#12675,#3304);
#2528=LINE('',#12678,#3305);
#2529=LINE('',#12679,#3306);
#2530=LINE('',#12682,#3307);
#2531=LINE('',#12683,#3308);
#2532=LINE('',#12685,#3309);
#2533=LINE('',#12688,#3310);
#2534=LINE('',#12689,#3311);
#2535=LINE('',#12692,#3312);
#2536=LINE('',#12693,#3313);
#2537=LINE('',#12696,#3314);
#2538=LINE('',#12697,#3315);
#2539=LINE('',#12700,#3316);
#2540=LINE('',#12701,#3317);
#2541=LINE('',#12703,#3318);
#2542=LINE('',#12709,#3319);
#2543=LINE('',#12711,#3320);
#2544=LINE('',#12713,#3321);
#2545=LINE('',#12714,#3322);
#2546=LINE('',#12717,#3323);
#2547=LINE('',#12719,#3324);
#2548=LINE('',#12720,#3325);
#2549=LINE('',#12723,#3326);
#2550=LINE('',#12725,#3327);
#2551=LINE('',#12726,#3328);
#2552=LINE('',#12729,#3329);
#2553=LINE('',#12731,#3330);
#2554=LINE('',#12732,#3331);
#2555=LINE('',#12735,#3332);
#2556=LINE('',#12737,#3333);
#2557=LINE('',#12738,#3334);
#2558=LINE('',#12741,#3335);
#2559=LINE('',#12743,#3336);
#2560=LINE('',#12744,#3337);
#2561=LINE('',#12747,#3338);
#2562=LINE('',#12749,#3339);
#2563=LINE('',#12750,#3340);
#2564=LINE('',#12752,#3341);
#2565=LINE('',#12753,#3342);
#2566=LINE('',#12760,#3343);
#2567=LINE('',#12762,#3344);
#2568=LINE('',#12764,#3345);
#2569=LINE('',#12765,#3346);
#2570=LINE('',#12768,#3347);
#2571=LINE('',#12770,#3348);
#2572=LINE('',#12771,#3349);
#2573=LINE('',#12774,#3350);
#2574=LINE('',#12776,#3351);
#2575=LINE('',#12777,#3352);
#2576=LINE('',#12780,#3353);
#2577=LINE('',#12782,#3354);
#2578=LINE('',#12783,#3355);
#2579=LINE('',#12786,#3356);
#2580=LINE('',#12788,#3357);
#2581=LINE('',#12789,#3358);
#2582=LINE('',#12792,#3359);
#2583=LINE('',#12794,#3360);
#2584=LINE('',#12795,#3361);
#2585=LINE('',#12798,#3362);
#2586=LINE('',#12800,#3363);
#2587=LINE('',#12801,#3364);
#2588=LINE('',#12803,#3365);
#2589=LINE('',#12804,#3366);
#2590=LINE('',#12814,#3367);
#2591=LINE('',#12816,#3368);
#2592=LINE('',#12818,#3369);
#2593=LINE('',#12819,#3370);
#2594=LINE('',#12822,#3371);
#2595=LINE('',#12824,#3372);
#2596=LINE('',#12825,#3373);
#2597=LINE('',#12828,#3374);
#2598=LINE('',#12830,#3375);
#2599=LINE('',#12831,#3376);
#2600=LINE('',#12834,#3377);
#2601=LINE('',#12836,#3378);
#2602=LINE('',#12837,#3379);
#2603=LINE('',#12840,#3380);
#2604=LINE('',#12842,#3381);
#2605=LINE('',#12843,#3382);
#2606=LINE('',#12845,#3383);
#2607=LINE('',#12846,#3384);
#2608=LINE('',#12858,#3385);
#2609=LINE('',#12862,#3386);
#2610=LINE('',#12866,#3387);
#2611=LINE('',#12873,#3388);
#2612=LINE('',#12875,#3389);
#2613=LINE('',#12883,#3390);
#2614=LINE('',#12887,#3391);
#2615=LINE('',#12891,#3392);
#2616=LINE('',#12898,#3393);
#2617=LINE('',#12902,#3394);
#2618=LINE('',#12906,#3395);
#2619=LINE('',#12911,#3396);
#2620=LINE('',#12913,#3397);
#2621=LINE('',#12915,#3398);
#2622=LINE('',#12916,#3399);
#2623=LINE('',#12919,#3400);
#2624=LINE('',#12921,#3401);
#2625=LINE('',#12922,#3402);
#2626=LINE('',#12925,#3403);
#2627=LINE('',#12927,#3404);
#2628=LINE('',#12928,#3405);
#2629=LINE('',#12931,#3406);
#2630=LINE('',#12933,#3407);
#2631=LINE('',#12934,#3408);
#2632=LINE('',#12937,#3409);
#2633=LINE('',#12939,#3410);
#2634=LINE('',#12940,#3411);
#2635=LINE('',#12942,#3412);
#2636=LINE('',#12943,#3413);
#2637=VECTOR('',#8708,0.274999999999999);
#2638=VECTOR('',#8715,0.275);
#2639=VECTOR('',#8722,0.275);
#2640=VECTOR('',#8729,0.274999999999999);
#2641=VECTOR('',#8734,1.);
#2642=VECTOR('',#8735,1.);
#2643=VECTOR('',#8736,1.);
#2644=VECTOR('',#8737,1.);
#2645=VECTOR('',#8740,1.);
#2646=VECTOR('',#8741,1.);
#2647=VECTOR('',#8742,1.);
#2648=VECTOR('',#8745,1.);
#2649=VECTOR('',#8746,1.);
#2650=VECTOR('',#8747,1.);
#2651=VECTOR('',#8750,1.);
#2652=VECTOR('',#8751,1.);
#2653=VECTOR('',#8762,0.274999999999999);
#2654=VECTOR('',#8769,0.275);
#2655=VECTOR('',#8776,0.275);
#2656=VECTOR('',#8783,0.274999999999999);
#2657=VECTOR('',#8788,1.);
#2658=VECTOR('',#8789,1.);
#2659=VECTOR('',#8790,1.);
#2660=VECTOR('',#8791,1.);
#2661=VECTOR('',#8794,1.);
#2662=VECTOR('',#8795,1.);
#2663=VECTOR('',#8796,1.);
#2664=VECTOR('',#8799,1.);
#2665=VECTOR('',#8800,1.);
#2666=VECTOR('',#8801,1.);
#2667=VECTOR('',#8804,1.);
#2668=VECTOR('',#8805,1.);
#2669=VECTOR('',#8808,1.);
#2670=VECTOR('',#8809,1.);
#2671=VECTOR('',#8810,1.);
#2672=VECTOR('',#8811,1.);
#2673=VECTOR('',#8814,1.);
#2674=VECTOR('',#8815,1.);
#2675=VECTOR('',#8816,1.);
#2676=VECTOR('',#8819,1.);
#2677=VECTOR('',#8820,1.);
#2678=VECTOR('',#8821,1.);
#2679=VECTOR('',#8824,1.);
#2680=VECTOR('',#8825,1.);
#2681=VECTOR('',#8834,1.);
#2682=VECTOR('',#8835,1.);
#2683=VECTOR('',#8836,1.);
#2684=VECTOR('',#8837,1.);
#2685=VECTOR('',#8840,1.);
#2686=VECTOR('',#8841,1.);
#2687=VECTOR('',#8842,1.);
#2688=VECTOR('',#8845,1.);
#2689=VECTOR('',#8846,1.);
#2690=VECTOR('',#8847,1.);
#2691=VECTOR('',#8850,1.);
#2692=VECTOR('',#8851,1.);
#2693=VECTOR('',#8860,1.);
#2694=VECTOR('',#8861,1.);
#2695=VECTOR('',#8862,1.);
#2696=VECTOR('',#8863,1.);
#2697=VECTOR('',#8866,1.);
#2698=VECTOR('',#8867,1.);
#2699=VECTOR('',#8868,1.);
#2700=VECTOR('',#8871,1.);
#2701=VECTOR('',#8872,1.);
#2702=VECTOR('',#8873,1.);
#2703=VECTOR('',#8876,1.);
#2704=VECTOR('',#8877,1.);
#2705=VECTOR('',#8886,1.);
#2706=VECTOR('',#8887,1.);
#2707=VECTOR('',#8888,1.);
#2708=VECTOR('',#8889,1.);
#2709=VECTOR('',#8892,1.);
#2710=VECTOR('',#8893,1.);
#2711=VECTOR('',#8894,1.);
#2712=VECTOR('',#8897,1.);
#2713=VECTOR('',#8898,1.);
#2714=VECTOR('',#8899,1.);
#2715=VECTOR('',#8902,1.);
#2716=VECTOR('',#8903,1.);
#2717=VECTOR('',#8914,0.225);
#2718=VECTOR('',#8921,0.225000000000001);
#2719=VECTOR('',#8926,1.);
#2720=VECTOR('',#8927,1.);
#2721=VECTOR('',#8928,1.);
#2722=VECTOR('',#8929,1.);
#2723=VECTOR('',#8932,1.);
#2724=VECTOR('',#8933,1.);
#2725=VECTOR('',#8934,1.);
#2726=VECTOR('',#8937,1.);
#2727=VECTOR('',#8938,1.);
#2728=VECTOR('',#8939,1.);
#2729=VECTOR('',#8942,1.);
#2730=VECTOR('',#8943,1.);
#2731=VECTOR('',#8954,0.225);
#2732=VECTOR('',#8961,0.225000000000001);
#2733=VECTOR('',#8966,1.);
#2734=VECTOR('',#8967,1.);
#2735=VECTOR('',#8968,1.);
#2736=VECTOR('',#8969,1.);
#2737=VECTOR('',#8972,1.);
#2738=VECTOR('',#8973,1.);
#2739=VECTOR('',#8974,1.);
#2740=VECTOR('',#8977,1.);
#2741=VECTOR('',#8978,1.);
#2742=VECTOR('',#8979,1.);
#2743=VECTOR('',#8982,1.);
#2744=VECTOR('',#8983,1.);
#2745=VECTOR('',#8994,0.165);
#2746=VECTOR('',#9003,0.5);
#2747=VECTOR('',#9014,0.275);
#2748=VECTOR('',#9017,1.);
#2749=VECTOR('',#9018,1.);
#2750=VECTOR('',#9019,1.);
#2751=VECTOR('',#9020,1.);
#2752=VECTOR('',#9023,1.);
#2753=VECTOR('',#9024,1.);
#2754=VECTOR('',#9025,1.);
#2755=VECTOR('',#9028,1.);
#2756=VECTOR('',#9029,1.);
#2757=VECTOR('',#9030,1.);
#2758=VECTOR('',#9033,1.);
#2759=VECTOR('',#9034,1.);
#2760=VECTOR('',#9045,0.165);
#2761=VECTOR('',#9054,0.5);
#2762=VECTOR('',#9063,0.275);
#2763=VECTOR('',#9068,1.);
#2764=VECTOR('',#9069,1.);
#2765=VECTOR('',#9070,1.);
#2766=VECTOR('',#9071,1.);
#2767=VECTOR('',#9074,1.);
#2768=VECTOR('',#9075,1.);
#2769=VECTOR('',#9076,1.);
#2770=VECTOR('',#9079,1.);
#2771=VECTOR('',#9080,1.);
#2772=VECTOR('',#9081,1.);
#2773=VECTOR('',#9084,1.);
#2774=VECTOR('',#9085,1.);
#2775=VECTOR('',#9096,0.164999999999999);
#2776=VECTOR('',#9105,0.5);
#2777=VECTOR('',#9116,0.274999999999999);
#2778=VECTOR('',#9119,1.);
#2779=VECTOR('',#9120,1.);
#2780=VECTOR('',#9121,1.);
#2781=VECTOR('',#9122,1.);
#2782=VECTOR('',#9125,1.);
#2783=VECTOR('',#9126,1.);
#2784=VECTOR('',#9127,1.);
#2785=VECTOR('',#9130,1.);
#2786=VECTOR('',#9131,1.);
#2787=VECTOR('',#9132,1.);
#2788=VECTOR('',#9135,1.);
#2789=VECTOR('',#9136,1.);
#2790=VECTOR('',#9147,0.164999999999999);
#2791=VECTOR('',#9156,0.5);
#2792=VECTOR('',#9165,0.274999999999999);
#2793=VECTOR('',#9170,1.);
#2794=VECTOR('',#9171,1.);
#2795=VECTOR('',#9172,1.);
#2796=VECTOR('',#9173,1.);
#2797=VECTOR('',#9176,1.);
#2798=VECTOR('',#9177,1.);
#2799=VECTOR('',#9178,1.);
#2800=VECTOR('',#9181,1.);
#2801=VECTOR('',#9182,1.);
#2802=VECTOR('',#9183,1.);
#2803=VECTOR('',#9186,1.);
#2804=VECTOR('',#9187,1.);
#2805=VECTOR('',#9196,1.);
#2806=VECTOR('',#9197,1.);
#2807=VECTOR('',#9198,1.);
#2808=VECTOR('',#9199,1.);
#2809=VECTOR('',#9202,1.);
#2810=VECTOR('',#9203,1.);
#2811=VECTOR('',#9204,1.);
#2812=VECTOR('',#9207,1.);
#2813=VECTOR('',#9208,1.);
#2814=VECTOR('',#9209,1.);
#2815=VECTOR('',#9212,1.);
#2816=VECTOR('',#9213,1.);
#2817=VECTOR('',#9216,1.);
#2818=VECTOR('',#9217,1.);
#2819=VECTOR('',#9218,1.);
#2820=VECTOR('',#9219,1.);
#2821=VECTOR('',#9222,1.);
#2822=VECTOR('',#9223,1.);
#2823=VECTOR('',#9224,1.);
#2824=VECTOR('',#9227,1.);
#2825=VECTOR('',#9228,1.);
#2826=VECTOR('',#9229,1.);
#2827=VECTOR('',#9232,1.);
#2828=VECTOR('',#9233,1.);
#2829=VECTOR('',#9242,1.);
#2830=VECTOR('',#9243,1.);
#2831=VECTOR('',#9244,1.);
#2832=VECTOR('',#9245,1.);
#2833=VECTOR('',#9248,1.);
#2834=VECTOR('',#9249,1.);
#2835=VECTOR('',#9250,1.);
#2836=VECTOR('',#9253,1.);
#2837=VECTOR('',#9254,1.);
#2838=VECTOR('',#9255,1.);
#2839=VECTOR('',#9258,1.);
#2840=VECTOR('',#9259,1.);
#2841=VECTOR('',#9262,1.);
#2842=VECTOR('',#9263,1.);
#2843=VECTOR('',#9264,1.);
#2844=VECTOR('',#9265,1.);
#2845=VECTOR('',#9268,1.);
#2846=VECTOR('',#9269,1.);
#2847=VECTOR('',#9270,1.);
#2848=VECTOR('',#9273,1.);
#2849=VECTOR('',#9274,1.);
#2850=VECTOR('',#9275,1.);
#2851=VECTOR('',#9278,1.);
#2852=VECTOR('',#9279,1.);
#2853=VECTOR('',#9290,0.210000000000001);
#2854=VECTOR('',#9297,0.21);
#2855=VECTOR('',#9304,0.164999999999999);
#2856=VECTOR('',#9311,0.164999999999999);
#2857=VECTOR('',#9318,0.164999999999999);
#2858=VECTOR('',#9325,0.164999999999999);
#2859=VECTOR('',#9332,0.275);
#2860=VECTOR('',#9339,0.274999999999999);
#2861=VECTOR('',#9344,1.);
#2862=VECTOR('',#9345,1.);
#2863=VECTOR('',#9346,1.);
#2864=VECTOR('',#9347,1.);
#2865=VECTOR('',#9350,1.);
#2866=VECTOR('',#9351,1.);
#2867=VECTOR('',#9352,1.);
#2868=VECTOR('',#9355,1.);
#2869=VECTOR('',#9356,1.);
#2870=VECTOR('',#9357,1.);
#2871=VECTOR('',#9360,1.);
#2872=VECTOR('',#9361,1.);
#2873=VECTOR('',#9372,0.225000000000001);
#2874=VECTOR('',#9379,0.225000000000001);
#2875=VECTOR('',#9384,1.);
#2876=VECTOR('',#9385,1.);
#2877=VECTOR('',#9386,1.);
#2878=VECTOR('',#9387,1.);
#2879=VECTOR('',#9390,1.);
#2880=VECTOR('',#9391,1.);
#2881=VECTOR('',#9392,1.);
#2882=VECTOR('',#9395,1.);
#2883=VECTOR('',#9396,1.);
#2884=VECTOR('',#9397,1.);
#2885=VECTOR('',#9400,1.);
#2886=VECTOR('',#9401,1.);
#2887=VECTOR('',#9402,1.);
#2888=VECTOR('',#9405,1.);
#2889=VECTOR('',#9406,1.);
#2890=VECTOR('',#9407,1.);
#2891=VECTOR('',#9410,1.);
#2892=VECTOR('',#9411,1.);
#2893=VECTOR('',#9422,0.164999999999999);
#2894=VECTOR('',#9431,0.274999999999999);
#2895=VECTOR('',#9436,1.);
#2896=VECTOR('',#9437,1.);
#2897=VECTOR('',#9438,1.);
#2898=VECTOR('',#9439,1.);
#2899=VECTOR('',#9442,1.);
#2900=VECTOR('',#9443,1.);
#2901=VECTOR('',#9444,1.);
#2902=VECTOR('',#9447,1.);
#2903=VECTOR('',#9448,1.);
#2904=VECTOR('',#9451,1.);
#2905=VECTOR('',#9452,1.);
#2906=VECTOR('',#9453,1.);
#2907=VECTOR('',#9454,1.);
#2908=VECTOR('',#9457,1.);
#2909=VECTOR('',#9458,1.);
#2910=VECTOR('',#9459,1.);
#2911=VECTOR('',#9462,1.);
#2912=VECTOR('',#9463,1.);
#2913=VECTOR('',#9466,1.);
#2914=VECTOR('',#9467,1.);
#2915=VECTOR('',#9470,1.);
#2916=VECTOR('',#9479,0.164999999999999);
#2917=VECTOR('',#9488,0.274999999999999);
#2918=VECTOR('',#9493,1.);
#2919=VECTOR('',#9494,1.);
#2920=VECTOR('',#9495,1.);
#2921=VECTOR('',#9496,1.);
#2922=VECTOR('',#9499,1.);
#2923=VECTOR('',#9500,1.);
#2924=VECTOR('',#9501,1.);
#2925=VECTOR('',#9504,1.);
#2926=VECTOR('',#9505,1.);
#2927=VECTOR('',#9508,1.);
#2928=VECTOR('',#9509,1.);
#2929=VECTOR('',#9510,1.);
#2930=VECTOR('',#9511,1.);
#2931=VECTOR('',#9514,1.);
#2932=VECTOR('',#9515,1.);
#2933=VECTOR('',#9516,1.);
#2934=VECTOR('',#9519,1.);
#2935=VECTOR('',#9520,1.);
#2936=VECTOR('',#9523,1.);
#2937=VECTOR('',#9524,1.);
#2938=VECTOR('',#9527,1.);
#2939=VECTOR('',#9536,0.275);
#2940=VECTOR('',#9541,1.);
#2941=VECTOR('',#9542,1.);
#2942=VECTOR('',#9543,1.);
#2943=VECTOR('',#9544,1.);
#2944=VECTOR('',#9547,1.);
#2945=VECTOR('',#9548,1.);
#2946=VECTOR('',#9549,1.);
#2947=VECTOR('',#9552,1.);
#2948=VECTOR('',#9553,1.);
#2949=VECTOR('',#9554,1.);
#2950=VECTOR('',#9557,1.);
#2951=VECTOR('',#9558,1.);
#2952=VECTOR('',#9569,0.274999999999999);
#2953=VECTOR('',#9574,1.);
#2954=VECTOR('',#9575,1.);
#2955=VECTOR('',#9576,1.);
#2956=VECTOR('',#9577,1.);
#2957=VECTOR('',#9580,1.);
#2958=VECTOR('',#9581,1.);
#2959=VECTOR('',#9582,1.);
#2960=VECTOR('',#9585,1.);
#2961=VECTOR('',#9586,1.);
#2962=VECTOR('',#9587,1.);
#2963=VECTOR('',#9590,1.);
#2964=VECTOR('',#9591,1.);
#2965=VECTOR('',#9600,1.);
#2966=VECTOR('',#9601,1.);
#2967=VECTOR('',#9602,1.);
#2968=VECTOR('',#9603,1.);
#2969=VECTOR('',#9606,1.);
#2970=VECTOR('',#9607,1.);
#2971=VECTOR('',#9608,1.);
#2972=VECTOR('',#9611,1.);
#2973=VECTOR('',#9612,1.);
#2974=VECTOR('',#9613,1.);
#2975=VECTOR('',#9616,1.);
#2976=VECTOR('',#9617,1.);
#2977=VECTOR('',#9618,1.);
#2978=VECTOR('',#9621,1.);
#2979=VECTOR('',#9622,1.);
#2980=VECTOR('',#9623,1.);
#2981=VECTOR('',#9626,1.);
#2982=VECTOR('',#9627,1.);
#2983=VECTOR('',#9628,1.);
#2984=VECTOR('',#9631,1.);
#2985=VECTOR('',#9632,1.);
#2986=VECTOR('',#9633,1.);
#2987=VECTOR('',#9636,1.);
#2988=VECTOR('',#9637,1.);
#2989=VECTOR('',#9638,1.);
#2990=VECTOR('',#9641,1.);
#2991=VECTOR('',#9642,1.);
#2992=VECTOR('',#9643,1.);
#2993=VECTOR('',#9646,1.);
#2994=VECTOR('',#9647,1.);
#2995=VECTOR('',#9648,1.);
#2996=VECTOR('',#9649,1.);
#2997=VECTOR('',#9652,1.);
#2998=VECTOR('',#9653,1.);
#2999=VECTOR('',#9654,1.);
#3000=VECTOR('',#9657,1.);
#3001=VECTOR('',#9658,1.);
#3002=VECTOR('',#9659,1.);
#3003=VECTOR('',#9662,1.);
#3004=VECTOR('',#9663,1.);
#3005=VECTOR('',#9664,1.);
#3006=VECTOR('',#9667,1.);
#3007=VECTOR('',#9668,1.);
#3008=VECTOR('',#9669,1.);
#3009=VECTOR('',#9672,1.);
#3010=VECTOR('',#9673,1.);
#3011=VECTOR('',#9674,1.);
#3012=VECTOR('',#9677,1.);
#3013=VECTOR('',#9678,1.);
#3014=VECTOR('',#9679,1.);
#3015=VECTOR('',#9682,1.);
#3016=VECTOR('',#9683,1.);
#3017=VECTOR('',#9684,1.);
#3018=VECTOR('',#9687,1.);
#3019=VECTOR('',#9688,1.);
#3020=VECTOR('',#9689,1.);
#3021=VECTOR('',#9692,1.);
#3022=VECTOR('',#9693,1.);
#3023=VECTOR('',#9694,1.);
#3024=VECTOR('',#9695,1.);
#3025=VECTOR('',#9698,1.);
#3026=VECTOR('',#9699,1.);
#3027=VECTOR('',#9700,1.);
#3028=VECTOR('',#9703,1.);
#3029=VECTOR('',#9704,1.);
#3030=VECTOR('',#9705,1.);
#3031=VECTOR('',#9708,1.);
#3032=VECTOR('',#9709,1.);
#3033=VECTOR('',#9710,1.);
#3034=VECTOR('',#9713,1.);
#3035=VECTOR('',#9714,1.);
#3036=VECTOR('',#9715,1.);
#3037=VECTOR('',#9718,1.);
#3038=VECTOR('',#9719,1.);
#3039=VECTOR('',#9720,1.);
#3040=VECTOR('',#9723,1.);
#3041=VECTOR('',#9724,1.);
#3042=VECTOR('',#9725,1.);
#3043=VECTOR('',#9728,1.);
#3044=VECTOR('',#9729,1.);
#3045=VECTOR('',#9730,1.);
#3046=VECTOR('',#9733,1.);
#3047=VECTOR('',#9734,1.);
#3048=VECTOR('',#9735,1.);
#3049=VECTOR('',#9738,1.);
#3050=VECTOR('',#9739,1.);
#3051=VECTOR('',#9740,1.);
#3052=VECTOR('',#9741,1.);
#3053=VECTOR('',#9744,1.);
#3054=VECTOR('',#9745,1.);
#3055=VECTOR('',#9746,1.);
#3056=VECTOR('',#9749,1.);
#3057=VECTOR('',#9750,1.);
#3058=VECTOR('',#9751,1.);
#3059=VECTOR('',#9754,1.);
#3060=VECTOR('',#9755,1.);
#3061=VECTOR('',#9756,1.);
#3062=VECTOR('',#9759,1.);
#3063=VECTOR('',#9760,1.);
#3064=VECTOR('',#9761,1.);
#3065=VECTOR('',#9764,1.);
#3066=VECTOR('',#9765,1.);
#3067=VECTOR('',#9766,1.);
#3068=VECTOR('',#9769,1.);
#3069=VECTOR('',#9770,1.);
#3070=VECTOR('',#9771,1.);
#3071=VECTOR('',#9774,1.);
#3072=VECTOR('',#9775,1.);
#3073=VECTOR('',#9776,1.);
#3074=VECTOR('',#9779,1.);
#3075=VECTOR('',#9780,1.);
#3076=VECTOR('',#9781,1.);
#3077=VECTOR('',#9786,0.21);
#3078=VECTOR('',#9791,1.);
#3079=VECTOR('',#9792,1.);
#3080=VECTOR('',#9793,1.);
#3081=VECTOR('',#9796,1.);
#3082=VECTOR('',#9797,1.);
#3083=VECTOR('',#9798,1.);
#3084=VECTOR('',#9801,1.);
#3085=VECTOR('',#9802,1.);
#3086=VECTOR('',#9805,1.);
#3087=VECTOR('',#9806,1.);
#3088=VECTOR('',#9807,1.);
#3089=VECTOR('',#9810,1.);
#3090=VECTOR('',#9811,1.);
#3091=VECTOR('',#9814,1.);
#3092=VECTOR('',#9815,1.);
#3093=VECTOR('',#9816,1.);
#3094=VECTOR('',#9819,1.);
#3095=VECTOR('',#9820,1.);
#3096=VECTOR('',#9823,1.);
#3097=VECTOR('',#9824,1.);
#3098=VECTOR('',#9839,0.4);
#3099=VECTOR('',#9844,0.425);
#3100=VECTOR('',#9849,0.41);
#3101=VECTOR('',#9858,0.26);
#3102=VECTOR('',#9863,0.25);
#3103=VECTOR('',#9868,0.225);
#3104=VECTOR('',#9873,1.);
#3105=VECTOR('',#9874,1.);
#3106=VECTOR('',#9875,1.);
#3107=VECTOR('',#9876,1.);
#3108=VECTOR('',#9879,1.);
#3109=VECTOR('',#9880,1.);
#3110=VECTOR('',#9881,1.);
#3111=VECTOR('',#9884,1.);
#3112=VECTOR('',#9885,1.);
#3113=VECTOR('',#9886,1.);
#3114=VECTOR('',#9889,1.);
#3115=VECTOR('',#9890,1.);
#3116=VECTOR('',#9891,1.);
#3117=VECTOR('',#9894,1.);
#3118=VECTOR('',#9895,1.);
#3119=VECTOR('',#9896,1.);
#3120=VECTOR('',#9899,1.);
#3121=VECTOR('',#9900,1.);
#3122=VECTOR('',#9911,0.375);
#3123=VECTOR('',#9922,0.375);
#3124=VECTOR('',#9933,0.375);
#3125=VECTOR('',#9944,0.375);
#3126=VECTOR('',#9955,0.225);
#3127=VECTOR('',#9960,0.225);
#3128=VECTOR('',#9965,0.225);
#3129=VECTOR('',#9970,0.225000000000001);
#3130=VECTOR('',#9973,1.);
#3131=VECTOR('',#9974,1.);
#3132=VECTOR('',#9975,1.);
#3133=VECTOR('',#9976,1.);
#3134=VECTOR('',#9979,1.);
#3135=VECTOR('',#9980,1.);
#3136=VECTOR('',#9981,1.);
#3137=VECTOR('',#9984,1.);
#3138=VECTOR('',#9985,1.);
#3139=VECTOR('',#9986,1.);
#3140=VECTOR('',#9989,1.);
#3141=VECTOR('',#9990,1.);
#3142=VECTOR('',#9991,1.);
#3143=VECTOR('',#9994,1.);
#3144=VECTOR('',#9995,1.);
#3145=VECTOR('',#9996,1.);
#3146=VECTOR('',#9999,1.);
#3147=VECTOR('',#10000,1.);
#3148=VECTOR('',#10001,1.);
#3149=VECTOR('',#10004,1.);
#3150=VECTOR('',#10005,1.);
#3151=VECTOR('',#10006,1.);
#3152=VECTOR('',#10009,1.);
#3153=VECTOR('',#10010,1.);
#3154=VECTOR('',#10011,1.);
#3155=VECTOR('',#10014,1.);
#3156=VECTOR('',#10015,1.);
#3157=VECTOR('',#10016,1.);
#3158=VECTOR('',#10019,1.);
#3159=VECTOR('',#10020,1.);
#3160=VECTOR('',#10021,1.);
#3161=VECTOR('',#10024,1.);
#3162=VECTOR('',#10025,1.);
#3163=VECTOR('',#10026,1.);
#3164=VECTOR('',#10029,1.);
#3165=VECTOR('',#10030,1.);
#3166=VECTOR('',#10039,1.);
#3167=VECTOR('',#10040,1.);
#3168=VECTOR('',#10041,1.);
#3169=VECTOR('',#10042,1.);
#3170=VECTOR('',#10045,1.);
#3171=VECTOR('',#10046,1.);
#3172=VECTOR('',#10047,1.);
#3173=VECTOR('',#10050,1.);
#3174=VECTOR('',#10051,1.);
#3175=VECTOR('',#10052,1.);
#3176=VECTOR('',#10057,1.);
#3177=VECTOR('',#10058,1.);
#3178=VECTOR('',#10059,1.);
#3179=VECTOR('',#10060,1.);
#3180=VECTOR('',#10061,1.);
#3181=VECTOR('',#10062,1.);
#3182=VECTOR('',#10063,1.);
#3183=VECTOR('',#10066,1.);
#3184=VECTOR('',#10067,1.);
#3185=VECTOR('',#10070,1.);
#3186=VECTOR('',#10071,1.);
#3187=VECTOR('',#10074,1.);
#3188=VECTOR('',#10075,1.);
#3189=VECTOR('',#10076,1.);
#3190=VECTOR('',#10077,1.);
#3191=VECTOR('',#10078,1.);
#3192=VECTOR('',#10081,1.);
#3193=VECTOR('',#10084,1.);
#3194=VECTOR('',#10087,1.);
#3195=VECTOR('',#10092,0.21);
#3196=VECTOR('',#10101,1.);
#3197=VECTOR('',#10104,1.);
#3198=VECTOR('',#10107,1.);
#3199=VECTOR('',#10116,0.275);
#3200=VECTOR('',#10121,0.265);
#3201=VECTOR('',#10130,0.5);
#3202=VECTOR('',#10139,1.);
#3203=VECTOR('',#10140,1.);
#3204=VECTOR('',#10141,1.);
#3205=VECTOR('',#10142,1.);
#3206=VECTOR('',#10145,1.);
#3207=VECTOR('',#10146,1.);
#3208=VECTOR('',#10147,1.);
#3209=VECTOR('',#10150,1.);
#3210=VECTOR('',#10151,1.);
#3211=VECTOR('',#10152,1.);
#3212=VECTOR('',#10155,1.);
#3213=VECTOR('',#10156,1.);
#3214=VECTOR('',#10157,1.);
#3215=VECTOR('',#10160,1.);
#3216=VECTOR('',#10161,1.);
#3217=VECTOR('',#10162,1.);
#3218=VECTOR('',#10165,1.);
#3219=VECTOR('',#10166,1.);
#3220=VECTOR('',#10179,0.25);
#3221=VECTOR('',#10192,0.4);
#3222=VECTOR('',#10197,0.425);
#3223=VECTOR('',#10202,0.41);
#3224=VECTOR('',#10211,0.26);
#3225=VECTOR('',#10214,0.25);
#3226=VECTOR('',#10223,0.225);
#3227=VECTOR('',#10230,0.225);
#3228=VECTOR('',#10237,0.275);
#3229=VECTOR('',#10244,0.275);
#3230=VECTOR('',#10251,0.275);
#3231=VECTOR('',#10258,0.275);
#3232=VECTOR('',#10263,1.);
#3233=VECTOR('',#10264,1.);
#3234=VECTOR('',#10265,1.);
#3235=VECTOR('',#10266,1.);
#3236=VECTOR('',#10269,1.);
#3237=VECTOR('',#10270,1.);
#3238=VECTOR('',#10271,1.);
#3239=VECTOR('',#10272,1.);
#3240=VECTOR('',#10275,1.);
#3241=VECTOR('',#10276,1.);
#3242=VECTOR('',#10279,1.);
#3243=VECTOR('',#10280,1.);
#3244=VECTOR('',#10281,1.);
#3245=VECTOR('',#10282,1.);
#3246=VECTOR('',#10283,1.);
#3247=VECTOR('',#10286,1.);
#3248=VECTOR('',#10287,1.);
#3249=VECTOR('',#10290,1.);
#3250=VECTOR('',#10291,1.);
#3251=VECTOR('',#10292,1.);
#3252=VECTOR('',#10295,1.);
#3253=VECTOR('',#10298,1.);
#3254=VECTOR('',#10299,1.);
#3255=VECTOR('',#10302,1.);
#3256=VECTOR('',#10311,0.164999999999999);
#3257=VECTOR('',#10320,0.164999999999999);
#3258=VECTOR('',#10329,0.5);
#3259=VECTOR('',#10338,1.);
#3260=VECTOR('',#10349,0.5);
#3261=VECTOR('',#10358,1.);
#3262=VECTOR('',#10367,0.5);
#3263=VECTOR('',#10374,1.);
#3264=VECTOR('',#10379,1.);
#3265=VECTOR('',#10382,0.21);
#3266=VECTOR('',#10387,1.);
#3267=VECTOR('',#10390,1.);
#3268=VECTOR('',#10395,1.);
#3269=VECTOR('',#10398,0.21);
#3270=VECTOR('',#10403,1.);
#3271=VECTOR('',#10406,1.);
#3272=VECTOR('',#10411,1.);
#3273=VECTOR('',#10414,0.21);
#3274=VECTOR('',#10419,1.);
#3275=VECTOR('',#10422,1.);
#3276=VECTOR('',#10427,1.);
#3277=VECTOR('',#10430,0.21);
#3278=VECTOR('',#10435,1.);
#3279=VECTOR('',#10438,1.);
#3280=VECTOR('',#10439,1.);
#3281=VECTOR('',#10440,1.);
#3282=VECTOR('',#10441,1.);
#3283=VECTOR('',#10442,1.);
#3284=VECTOR('',#10443,1.);
#3285=VECTOR('',#10446,1.);
#3286=VECTOR('',#10447,1.);
#3287=VECTOR('',#10448,1.);
#3288=VECTOR('',#10449,1.);
#3289=VECTOR('',#10450,1.);
#3290=VECTOR('',#10451,1.);
#3291=VECTOR('',#10454,1.);
#3292=VECTOR('',#10455,1.);
#3293=VECTOR('',#10456,1.);
#3294=VECTOR('',#10457,1.);
#3295=VECTOR('',#10458,1.);
#3296=VECTOR('',#10459,1.);
#3297=VECTOR('',#10460,1.);
#3298=VECTOR('',#10461,1.);
#3299=VECTOR('',#10462,1.);
#3300=VECTOR('',#10463,1.);
#3301=VECTOR('',#10466,1.);
#3302=VECTOR('',#10467,1.);
#3303=VECTOR('',#10470,1.);
#3304=VECTOR('',#10471,1.);
#3305=VECTOR('',#10474,1.);
#3306=VECTOR('',#10475,1.);
#3307=VECTOR('',#10478,1.);
#3308=VECTOR('',#10479,1.);
#3309=VECTOR('',#10482,1.);
#3310=VECTOR('',#10485,1.);
#3311=VECTOR('',#10486,1.);
#3312=VECTOR('',#10489,1.);
#3313=VECTOR('',#10490,1.);
#3314=VECTOR('',#10493,1.);
#3315=VECTOR('',#10494,1.);
#3316=VECTOR('',#10497,1.);
#3317=VECTOR('',#10498,1.);
#3318=VECTOR('',#10501,1.);
#3319=VECTOR('',#10508,1.);
#3320=VECTOR('',#10509,1.);
#3321=VECTOR('',#10510,1.);
#3322=VECTOR('',#10511,1.);
#3323=VECTOR('',#10514,1.);
#3324=VECTOR('',#10515,1.);
#3325=VECTOR('',#10516,1.);
#3326=VECTOR('',#10519,1.);
#3327=VECTOR('',#10520,1.);
#3328=VECTOR('',#10521,1.);
#3329=VECTOR('',#10524,1.);
#3330=VECTOR('',#10525,1.);
#3331=VECTOR('',#10526,1.);
#3332=VECTOR('',#10529,1.);
#3333=VECTOR('',#10530,1.);
#3334=VECTOR('',#10531,1.);
#3335=VECTOR('',#10534,1.);
#3336=VECTOR('',#10535,1.);
#3337=VECTOR('',#10536,1.);
#3338=VECTOR('',#10539,1.);
#3339=VECTOR('',#10540,1.);
#3340=VECTOR('',#10541,1.);
#3341=VECTOR('',#10544,1.);
#3342=VECTOR('',#10545,1.);
#3343=VECTOR('',#10554,1.);
#3344=VECTOR('',#10555,1.);
#3345=VECTOR('',#10556,1.);
#3346=VECTOR('',#10557,1.);
#3347=VECTOR('',#10560,1.);
#3348=VECTOR('',#10561,1.);
#3349=VECTOR('',#10562,1.);
#3350=VECTOR('',#10565,1.);
#3351=VECTOR('',#10566,1.);
#3352=VECTOR('',#10567,1.);
#3353=VECTOR('',#10570,1.);
#3354=VECTOR('',#10571,1.);
#3355=VECTOR('',#10572,1.);
#3356=VECTOR('',#10575,1.);
#3357=VECTOR('',#10576,1.);
#3358=VECTOR('',#10577,1.);
#3359=VECTOR('',#10580,1.);
#3360=VECTOR('',#10581,1.);
#3361=VECTOR('',#10582,1.);
#3362=VECTOR('',#10585,1.);
#3363=VECTOR('',#10586,1.);
#3364=VECTOR('',#10587,1.);
#3365=VECTOR('',#10590,1.);
#3366=VECTOR('',#10591,1.);
#3367=VECTOR('',#10606,1.);
#3368=VECTOR('',#10607,1.);
#3369=VECTOR('',#10608,1.);
#3370=VECTOR('',#10609,1.);
#3371=VECTOR('',#10612,1.);
#3372=VECTOR('',#10613,1.);
#3373=VECTOR('',#10614,1.);
#3374=VECTOR('',#10617,1.);
#3375=VECTOR('',#10618,1.);
#3376=VECTOR('',#10619,1.);
#3377=VECTOR('',#10622,1.);
#3378=VECTOR('',#10623,1.);
#3379=VECTOR('',#10624,1.);
#3380=VECTOR('',#10627,1.);
#3381=VECTOR('',#10628,1.);
#3382=VECTOR('',#10629,1.);
#3383=VECTOR('',#10632,1.);
#3384=VECTOR('',#10633,1.);
#3385=VECTOR('',#10650,0.4);
#3386=VECTOR('',#10655,0.425);
#3387=VECTOR('',#10660,0.41);
#3388=VECTOR('',#10669,0.26);
#3389=VECTOR('',#10672,0.25);
#3390=VECTOR('',#10683,0.325);
#3391=VECTOR('',#10688,0.35);
#3392=VECTOR('',#10693,0.335);
#3393=VECTOR('',#10702,0.21);
#3394=VECTOR('',#10707,0.2);
#3395=VECTOR('',#10712,0.18);
#3396=VECTOR('',#10717,1.);
#3397=VECTOR('',#10718,1.);
#3398=VECTOR('',#10719,1.);
#3399=VECTOR('',#10720,1.);
#3400=VECTOR('',#10723,1.);
#3401=VECTOR('',#10724,1.);
#3402=VECTOR('',#10725,1.);
#3403=VECTOR('',#10728,1.);
#3404=VECTOR('',#10729,1.);
#3405=VECTOR('',#10730,1.);
#3406=VECTOR('',#10733,1.);
#3407=VECTOR('',#10734,1.);
#3408=VECTOR('',#10735,1.);
#3409=VECTOR('',#10738,1.);
#3410=VECTOR('',#10739,1.);
#3411=VECTOR('',#10740,1.);
#3412=VECTOR('',#10743,1.);
#3413=VECTOR('',#10744,1.);
#3414=CIRCLE('',#7990,0.274999999999999);
#3415=CIRCLE('',#7991,0.274999999999999);
#3416=CIRCLE('',#7993,0.275);
#3417=CIRCLE('',#7994,0.275);
#3418=CIRCLE('',#7996,0.275);
#3419=CIRCLE('',#7997,0.275);
#3420=CIRCLE('',#7999,0.274999999999999);
#3421=CIRCLE('',#8000,0.274999999999999);
#3422=CIRCLE('',#8009,0.274999999999999);
#3423=CIRCLE('',#8010,0.274999999999999);
#3424=CIRCLE('',#8012,0.275);
#3425=CIRCLE('',#8013,0.275);
#3426=CIRCLE('',#8015,0.275);
#3427=CIRCLE('',#8016,0.275);
#3428=CIRCLE('',#8018,0.274999999999999);
#3429=CIRCLE('',#8019,0.274999999999999);
#3430=CIRCLE('',#8053,0.225);
#3431=CIRCLE('',#8054,0.225);
#3432=CIRCLE('',#8056,0.225000000000001);
#3433=CIRCLE('',#8057,0.225000000000001);
#3434=CIRCLE('',#8066,0.225);
#3435=CIRCLE('',#8067,0.225);
#3436=CIRCLE('',#8069,0.225000000000001);
#3437=CIRCLE('',#8070,0.225000000000001);
#3438=CIRCLE('',#8079,0.165);
#3439=CIRCLE('',#8080,0.165);
#3440=CIRCLE('',#8083,0.5);
#3441=CIRCLE('',#8084,0.5);
#3442=CIRCLE('',#8086,0.275);
#3443=CIRCLE('',#8088,0.275);
#3444=CIRCLE('',#8097,0.165);
#3445=CIRCLE('',#8098,0.165);
#3446=CIRCLE('',#8101,0.5);
#3447=CIRCLE('',#8102,0.5);
#3448=CIRCLE('',#8104,0.275);
#3449=CIRCLE('',#8106,0.275);
#3450=CIRCLE('',#8115,0.164999999999999);
#3451=CIRCLE('',#8116,0.164999999999999);
#3452=CIRCLE('',#8119,0.5);
#3453=CIRCLE('',#8120,0.5);
#3454=CIRCLE('',#8122,0.274999999999999);
#3455=CIRCLE('',#8124,0.274999999999999);
#3456=CIRCLE('',#8133,0.164999999999999);
#3457=CIRCLE('',#8134,0.164999999999999);
#3458=CIRCLE('',#8137,0.5);
#3459=CIRCLE('',#8138,0.5);
#3460=CIRCLE('',#8140,0.274999999999999);
#3461=CIRCLE('',#8142,0.274999999999999);
#3462=CIRCLE('',#8173,0.210000000000001);
#3463=CIRCLE('',#8174,0.210000000000001);
#3464=CIRCLE('',#8176,0.21);
#3465=CIRCLE('',#8177,0.21);
#3466=CIRCLE('',#8179,0.164999999999999);
#3467=CIRCLE('',#8180,0.164999999999999);
#3468=CIRCLE('',#8182,0.164999999999999);
#3469=CIRCLE('',#8183,0.164999999999999);
#3470=CIRCLE('',#8185,0.164999999999999);
#3471=CIRCLE('',#8186,0.164999999999999);
#3472=CIRCLE('',#8188,0.164999999999999);
#3473=CIRCLE('',#8189,0.164999999999999);
#3474=CIRCLE('',#8191,0.275);
#3475=CIRCLE('',#8192,0.275);
#3476=CIRCLE('',#8194,0.274999999999999);
#3477=CIRCLE('',#8195,0.274999999999999);
#3478=CIRCLE('',#8204,0.225000000000001);
#3479=CIRCLE('',#8205,0.225000000000001);
#3480=CIRCLE('',#8207,0.225000000000001);
#3481=CIRCLE('',#8208,0.225000000000001);
#3482=CIRCLE('',#8219,0.164999999999999);
#3483=CIRCLE('',#8220,0.164999999999999);
#3484=CIRCLE('',#8223,0.274999999999999);
#3485=CIRCLE('',#8224,0.274999999999999);
#3486=CIRCLE('',#8236,0.164999999999999);
#3487=CIRCLE('',#8237,0.164999999999999);
#3488=CIRCLE('',#8240,0.274999999999999);
#3489=CIRCLE('',#8241,0.274999999999999);
#3490=CIRCLE('',#8253,0.275);
#3491=CIRCLE('',#8254,0.275);
#3492=CIRCLE('',#8263,0.274999999999999);
#3493=CIRCLE('',#8264,0.274999999999999);
#3494=CIRCLE('',#8309,0.21);
#3495=CIRCLE('',#8310,0.21);
#3496=CIRCLE('',#8323,0.375);
#3497=CIRCLE('',#8325,0.425);
#3498=CIRCLE('',#8327,0.425);
#3499=CIRCLE('',#8329,0.395);
#3500=CIRCLE('',#8331,0.27);
#3501=CIRCLE('',#8333,0.24505);
#3502=CIRCLE('',#8335,0.24505);
#3503=CIRCLE('',#8337,0.2);
#3504=CIRCLE('',#8349,0.375);
#3505=CIRCLE('',#8350,0.375);
#3506=CIRCLE('',#8352,0.225);
#3507=CIRCLE('',#8354,0.375);
#3508=CIRCLE('',#8355,0.375);
#3509=CIRCLE('',#8357,0.225);
#3510=CIRCLE('',#8359,0.375);
#3511=CIRCLE('',#8360,0.375);
#3512=CIRCLE('',#8362,0.225);
#3513=CIRCLE('',#8364,0.375);
#3514=CIRCLE('',#8365,0.375);
#3515=CIRCLE('',#8367,0.225000000000001);
#3516=CIRCLE('',#8369,0.225);
#3517=CIRCLE('',#8371,0.225);
#3518=CIRCLE('',#8373,0.225);
#3519=CIRCLE('',#8375,0.225000000000001);
#3520=CIRCLE('',#8394,0.2117);
#3521=CIRCLE('',#8403,0.2117);
#3522=CIRCLE('',#8404,0.2117);
#3523=CIRCLE('',#8406,0.2117);
#3524=CIRCLE('',#8413,0.285);
#3525=CIRCLE('',#8414,0.265);
#3526=CIRCLE('',#8416,0.265);
#3527=CIRCLE('',#8418,0.5);
#3528=CIRCLE('',#8420,0.5);
#3529=CIRCLE('',#8432,0.25);
#3530=CIRCLE('',#8433,0.24505);
#3531=CIRCLE('',#8435,0.25);
#3532=CIRCLE('',#8438,0.375);
#3533=CIRCLE('',#8440,0.425);
#3534=CIRCLE('',#8442,0.425);
#3535=CIRCLE('',#8444,0.395);
#3536=CIRCLE('',#8446,0.27);
#3537=CIRCLE('',#8448,0.24505);
#3538=CIRCLE('',#8453,0.225);
#3539=CIRCLE('',#8454,0.225);
#3540=CIRCLE('',#8456,0.225);
#3541=CIRCLE('',#8457,0.225);
#3542=CIRCLE('',#8459,0.275);
#3543=CIRCLE('',#8460,0.275);
#3544=CIRCLE('',#8462,0.275);
#3545=CIRCLE('',#8463,0.275);
#3546=CIRCLE('',#8465,0.275);
#3547=CIRCLE('',#8466,0.275);
#3548=CIRCLE('',#8468,0.275);
#3549=CIRCLE('',#8469,0.275);
#3550=CIRCLE('',#8482,0.164999999999999);
#3551=CIRCLE('',#8483,0.164999999999999);
#3552=CIRCLE('',#8486,0.164999999999999);
#3553=CIRCLE('',#8487,0.164999999999999);
#3554=CIRCLE('',#8490,0.5);
#3555=CIRCLE('',#8492,0.5);
#3556=CIRCLE('',#8496,0.5);
#3557=CIRCLE('',#8497,0.5);
#3558=CIRCLE('',#8499,0.5);
#3559=CIRCLE('',#8500,0.5);
#3560=CIRCLE('',#8505,0.5);
#3561=CIRCLE('',#8506,0.5);
#3562=CIRCLE('',#8511,0.21);
#3563=CIRCLE('',#8513,0.21);
#3564=CIRCLE('',#8514,0.21);
#3565=CIRCLE('',#8515,0.21);
#3566=CIRCLE('',#8517,0.21);
#3567=CIRCLE('',#8519,0.21);
#3568=CIRCLE('',#8520,0.21);
#3569=CIRCLE('',#8521,0.21);
#3570=CIRCLE('',#8523,0.21);
#3571=CIRCLE('',#8525,0.21);
#3572=CIRCLE('',#8526,0.21);
#3573=CIRCLE('',#8527,0.21);
#3574=CIRCLE('',#8529,0.21);
#3575=CIRCLE('',#8531,0.21);
#3576=CIRCLE('',#8532,0.21);
#3577=CIRCLE('',#8533,0.21);
#3578=CIRCLE('',#8583,0.24505);
#3579=CIRCLE('',#8585,0.375);
#3580=CIRCLE('',#8587,0.425);
#3581=CIRCLE('',#8589,0.425);
#3582=CIRCLE('',#8591,0.395);
#3583=CIRCLE('',#8593,0.27);
#3584=CIRCLE('',#8595,0.24505);
#3585=CIRCLE('',#8599,0.3);
#3586=CIRCLE('',#8601,0.35);
#3587=CIRCLE('',#8603,0.35);
#3588=CIRCLE('',#8605,0.32);
#3589=CIRCLE('',#8607,0.22);
#3590=CIRCLE('',#8609,0.1954);
#3591=CIRCLE('',#8611,0.1954);
#3592=CIRCLE('',#8613,0.16);
#3593=VERTEX_POINT('',#10903);
#3594=VERTEX_POINT('',#10905);
#3595=VERTEX_POINT('',#10909);
#3596=VERTEX_POINT('',#10911);
#3597=VERTEX_POINT('',#10915);
#3598=VERTEX_POINT('',#10917);
#3599=VERTEX_POINT('',#10921);
#3600=VERTEX_POINT('',#10923);
#3601=VERTEX_POINT('',#10927);
#3602=VERTEX_POINT('',#10928);
#3603=VERTEX_POINT('',#10930);
#3604=VERTEX_POINT('',#10932);
#3605=VERTEX_POINT('',#10936);
#3606=VERTEX_POINT('',#10938);
#3607=VERTEX_POINT('',#10942);
#3608=VERTEX_POINT('',#10944);
#3609=VERTEX_POINT('',#10954);
#3610=VERTEX_POINT('',#10956);
#3611=VERTEX_POINT('',#10960);
#3612=VERTEX_POINT('',#10962);
#3613=VERTEX_POINT('',#10966);
#3614=VERTEX_POINT('',#10968);
#3615=VERTEX_POINT('',#10972);
#3616=VERTEX_POINT('',#10974);
#3617=VERTEX_POINT('',#10978);
#3618=VERTEX_POINT('',#10979);
#3619=VERTEX_POINT('',#10981);
#3620=VERTEX_POINT('',#10983);
#3621=VERTEX_POINT('',#10987);
#3622=VERTEX_POINT('',#10989);
#3623=VERTEX_POINT('',#10993);
#3624=VERTEX_POINT('',#10995);
#3625=VERTEX_POINT('',#11002);
#3626=VERTEX_POINT('',#11003);
#3627=VERTEX_POINT('',#11005);
#3628=VERTEX_POINT('',#11007);
#3629=VERTEX_POINT('',#11011);
#3630=VERTEX_POINT('',#11013);
#3631=VERTEX_POINT('',#11017);
#3632=VERTEX_POINT('',#11019);
#3633=VERTEX_POINT('',#11029);
#3634=VERTEX_POINT('',#11030);
#3635=VERTEX_POINT('',#11032);
#3636=VERTEX_POINT('',#11034);
#3637=VERTEX_POINT('',#11038);
#3638=VERTEX_POINT('',#11040);
#3639=VERTEX_POINT('',#11044);
#3640=VERTEX_POINT('',#11046);
#3641=VERTEX_POINT('',#11056);
#3642=VERTEX_POINT('',#11057);
#3643=VERTEX_POINT('',#11059);
#3644=VERTEX_POINT('',#11061);
#3645=VERTEX_POINT('',#11065);
#3646=VERTEX_POINT('',#11067);
#3647=VERTEX_POINT('',#11071);
#3648=VERTEX_POINT('',#11073);
#3649=VERTEX_POINT('',#11083);
#3650=VERTEX_POINT('',#11084);
#3651=VERTEX_POINT('',#11086);
#3652=VERTEX_POINT('',#11088);
#3653=VERTEX_POINT('',#11092);
#3654=VERTEX_POINT('',#11094);
#3655=VERTEX_POINT('',#11098);
#3656=VERTEX_POINT('',#11100);
#3657=VERTEX_POINT('',#11110);
#3658=VERTEX_POINT('',#11112);
#3659=VERTEX_POINT('',#11116);
#3660=VERTEX_POINT('',#11118);
#3661=VERTEX_POINT('',#11122);
#3662=VERTEX_POINT('',#11123);
#3663=VERTEX_POINT('',#11125);
#3664=VERTEX_POINT('',#11127);
#3665=VERTEX_POINT('',#11131);
#3666=VERTEX_POINT('',#11133);
#3667=VERTEX_POINT('',#11137);
#3668=VERTEX_POINT('',#11139);
#3669=VERTEX_POINT('',#11149);
#3670=VERTEX_POINT('',#11151);
#3671=VERTEX_POINT('',#11155);
#3672=VERTEX_POINT('',#11157);
#3673=VERTEX_POINT('',#11161);
#3674=VERTEX_POINT('',#11162);
#3675=VERTEX_POINT('',#11164);
#3676=VERTEX_POINT('',#11166);
#3677=VERTEX_POINT('',#11170);
#3678=VERTEX_POINT('',#11172);
#3679=VERTEX_POINT('',#11176);
#3680=VERTEX_POINT('',#11178);
#3681=VERTEX_POINT('',#11188);
#3682=VERTEX_POINT('',#11190);
#3683=VERTEX_POINT('',#11195);
#3684=VERTEX_POINT('',#11197);
#3685=VERTEX_POINT('',#11201);
#3686=VERTEX_POINT('',#11204);
#3687=VERTEX_POINT('',#11208);
#3688=VERTEX_POINT('',#11209);
#3689=VERTEX_POINT('',#11211);
#3690=VERTEX_POINT('',#11213);
#3691=VERTEX_POINT('',#11217);
#3692=VERTEX_POINT('',#11219);
#3693=VERTEX_POINT('',#11223);
#3694=VERTEX_POINT('',#11225);
#3695=VERTEX_POINT('',#11235);
#3696=VERTEX_POINT('',#11237);
#3697=VERTEX_POINT('',#11242);
#3698=VERTEX_POINT('',#11244);
#3699=VERTEX_POINT('',#11248);
#3700=VERTEX_POINT('',#11251);
#3701=VERTEX_POINT('',#11255);
#3702=VERTEX_POINT('',#11256);
#3703=VERTEX_POINT('',#11258);
#3704=VERTEX_POINT('',#11260);
#3705=VERTEX_POINT('',#11264);
#3706=VERTEX_POINT('',#11266);
#3707=VERTEX_POINT('',#11270);
#3708=VERTEX_POINT('',#11272);
#3709=VERTEX_POINT('',#11282);
#3710=VERTEX_POINT('',#11284);
#3711=VERTEX_POINT('',#11289);
#3712=VERTEX_POINT('',#11291);
#3713=VERTEX_POINT('',#11295);
#3714=VERTEX_POINT('',#11298);
#3715=VERTEX_POINT('',#11302);
#3716=VERTEX_POINT('',#11303);
#3717=VERTEX_POINT('',#11305);
#3718=VERTEX_POINT('',#11307);
#3719=VERTEX_POINT('',#11311);
#3720=VERTEX_POINT('',#11313);
#3721=VERTEX_POINT('',#11317);
#3722=VERTEX_POINT('',#11319);
#3723=VERTEX_POINT('',#11329);
#3724=VERTEX_POINT('',#11331);
#3725=VERTEX_POINT('',#11336);
#3726=VERTEX_POINT('',#11338);
#3727=VERTEX_POINT('',#11342);
#3728=VERTEX_POINT('',#11345);
#3729=VERTEX_POINT('',#11349);
#3730=VERTEX_POINT('',#11350);
#3731=VERTEX_POINT('',#11352);
#3732=VERTEX_POINT('',#11354);
#3733=VERTEX_POINT('',#11358);
#3734=VERTEX_POINT('',#11360);
#3735=VERTEX_POINT('',#11364);
#3736=VERTEX_POINT('',#11366);
#3737=VERTEX_POINT('',#11376);
#3738=VERTEX_POINT('',#11377);
#3739=VERTEX_POINT('',#11379);
#3740=VERTEX_POINT('',#11381);
#3741=VERTEX_POINT('',#11385);
#3742=VERTEX_POINT('',#11387);
#3743=VERTEX_POINT('',#11391);
#3744=VERTEX_POINT('',#11393);
#3745=VERTEX_POINT('',#11400);
#3746=VERTEX_POINT('',#11401);
#3747=VERTEX_POINT('',#11403);
#3748=VERTEX_POINT('',#11405);
#3749=VERTEX_POINT('',#11409);
#3750=VERTEX_POINT('',#11411);
#3751=VERTEX_POINT('',#11415);
#3752=VERTEX_POINT('',#11417);
#3753=VERTEX_POINT('',#11427);
#3754=VERTEX_POINT('',#11428);
#3755=VERTEX_POINT('',#11430);
#3756=VERTEX_POINT('',#11432);
#3757=VERTEX_POINT('',#11436);
#3758=VERTEX_POINT('',#11438);
#3759=VERTEX_POINT('',#11442);
#3760=VERTEX_POINT('',#11444);
#3761=VERTEX_POINT('',#11451);
#3762=VERTEX_POINT('',#11452);
#3763=VERTEX_POINT('',#11454);
#3764=VERTEX_POINT('',#11456);
#3765=VERTEX_POINT('',#11460);
#3766=VERTEX_POINT('',#11462);
#3767=VERTEX_POINT('',#11466);
#3768=VERTEX_POINT('',#11468);
#3769=VERTEX_POINT('',#11478);
#3770=VERTEX_POINT('',#11480);
#3771=VERTEX_POINT('',#11484);
#3772=VERTEX_POINT('',#11486);
#3773=VERTEX_POINT('',#11490);
#3774=VERTEX_POINT('',#11492);
#3775=VERTEX_POINT('',#11496);
#3776=VERTEX_POINT('',#11498);
#3777=VERTEX_POINT('',#11502);
#3778=VERTEX_POINT('',#11504);
#3779=VERTEX_POINT('',#11508);
#3780=VERTEX_POINT('',#11510);
#3781=VERTEX_POINT('',#11514);
#3782=VERTEX_POINT('',#11516);
#3783=VERTEX_POINT('',#11520);
#3784=VERTEX_POINT('',#11522);
#3785=VERTEX_POINT('',#11526);
#3786=VERTEX_POINT('',#11527);
#3787=VERTEX_POINT('',#11529);
#3788=VERTEX_POINT('',#11531);
#3789=VERTEX_POINT('',#11535);
#3790=VERTEX_POINT('',#11537);
#3791=VERTEX_POINT('',#11541);
#3792=VERTEX_POINT('',#11543);
#3793=VERTEX_POINT('',#11553);
#3794=VERTEX_POINT('',#11555);
#3795=VERTEX_POINT('',#11559);
#3796=VERTEX_POINT('',#11561);
#3797=VERTEX_POINT('',#11565);
#3798=VERTEX_POINT('',#11566);
#3799=VERTEX_POINT('',#11568);
#3800=VERTEX_POINT('',#11570);
#3801=VERTEX_POINT('',#11574);
#3802=VERTEX_POINT('',#11576);
#3803=VERTEX_POINT('',#11580);
#3804=VERTEX_POINT('',#11582);
#3805=VERTEX_POINT('',#11586);
#3806=VERTEX_POINT('',#11588);
#3807=VERTEX_POINT('',#11592);
#3808=VERTEX_POINT('',#11594);
#3809=VERTEX_POINT('',#11604);
#3810=VERTEX_POINT('',#11606);
#3811=VERTEX_POINT('',#11611);
#3812=VERTEX_POINT('',#11613);
#3813=VERTEX_POINT('',#11617);
#3814=VERTEX_POINT('',#11618);
#3815=VERTEX_POINT('',#11620);
#3816=VERTEX_POINT('',#11622);
#3817=VERTEX_POINT('',#11626);
#3818=VERTEX_POINT('',#11628);
#3819=VERTEX_POINT('',#11632);
#3820=VERTEX_POINT('',#11636);
#3821=VERTEX_POINT('',#11638);
#3822=VERTEX_POINT('',#11640);
#3823=VERTEX_POINT('',#11644);
#3824=VERTEX_POINT('',#11646);
#3825=VERTEX_POINT('',#11650);
#3826=VERTEX_POINT('',#11654);
#3827=VERTEX_POINT('',#11662);
#3828=VERTEX_POINT('',#11664);
#3829=VERTEX_POINT('',#11669);
#3830=VERTEX_POINT('',#11671);
#3831=VERTEX_POINT('',#11675);
#3832=VERTEX_POINT('',#11676);
#3833=VERTEX_POINT('',#11678);
#3834=VERTEX_POINT('',#11680);
#3835=VERTEX_POINT('',#11684);
#3836=VERTEX_POINT('',#11686);
#3837=VERTEX_POINT('',#11690);
#3838=VERTEX_POINT('',#11694);
#3839=VERTEX_POINT('',#11696);
#3840=VERTEX_POINT('',#11698);
#3841=VERTEX_POINT('',#11702);
#3842=VERTEX_POINT('',#11704);
#3843=VERTEX_POINT('',#11708);
#3844=VERTEX_POINT('',#11712);
#3845=VERTEX_POINT('',#11720);
#3846=VERTEX_POINT('',#11722);
#3847=VERTEX_POINT('',#11726);
#3848=VERTEX_POINT('',#11727);
#3849=VERTEX_POINT('',#11729);
#3850=VERTEX_POINT('',#11731);
#3851=VERTEX_POINT('',#11735);
#3852=VERTEX_POINT('',#11737);
#3853=VERTEX_POINT('',#11741);
#3854=VERTEX_POINT('',#11743);
#3855=VERTEX_POINT('',#11753);
#3856=VERTEX_POINT('',#11755);
#3857=VERTEX_POINT('',#11759);
#3858=VERTEX_POINT('',#11760);
#3859=VERTEX_POINT('',#11762);
#3860=VERTEX_POINT('',#11764);
#3861=VERTEX_POINT('',#11768);
#3862=VERTEX_POINT('',#11770);
#3863=VERTEX_POINT('',#11774);
#3864=VERTEX_POINT('',#11776);
#3865=VERTEX_POINT('',#11786);
#3866=VERTEX_POINT('',#11787);
#3867=VERTEX_POINT('',#11789);
#3868=VERTEX_POINT('',#11791);
#3869=VERTEX_POINT('',#11795);
#3870=VERTEX_POINT('',#11797);
#3871=VERTEX_POINT('',#11801);
#3872=VERTEX_POINT('',#11803);
#3873=VERTEX_POINT('',#11807);
#3874=VERTEX_POINT('',#11809);
#3875=VERTEX_POINT('',#11813);
#3876=VERTEX_POINT('',#11815);
#3877=VERTEX_POINT('',#11819);
#3878=VERTEX_POINT('',#11821);
#3879=VERTEX_POINT('',#11825);
#3880=VERTEX_POINT('',#11827);
#3881=VERTEX_POINT('',#11831);
#3882=VERTEX_POINT('',#11833);
#3883=VERTEX_POINT('',#11837);
#3884=VERTEX_POINT('',#11839);
#3885=VERTEX_POINT('',#11843);
#3886=VERTEX_POINT('',#11844);
#3887=VERTEX_POINT('',#11846);
#3888=VERTEX_POINT('',#11848);
#3889=VERTEX_POINT('',#11852);
#3890=VERTEX_POINT('',#11854);
#3891=VERTEX_POINT('',#11858);
#3892=VERTEX_POINT('',#11860);
#3893=VERTEX_POINT('',#11864);
#3894=VERTEX_POINT('',#11866);
#3895=VERTEX_POINT('',#11870);
#3896=VERTEX_POINT('',#11872);
#3897=VERTEX_POINT('',#11876);
#3898=VERTEX_POINT('',#11878);
#3899=VERTEX_POINT('',#11882);
#3900=VERTEX_POINT('',#11884);
#3901=VERTEX_POINT('',#11888);
#3902=VERTEX_POINT('',#11890);
#3903=VERTEX_POINT('',#11894);
#3904=VERTEX_POINT('',#11896);
#3905=VERTEX_POINT('',#11900);
#3906=VERTEX_POINT('',#11901);
#3907=VERTEX_POINT('',#11903);
#3908=VERTEX_POINT('',#11905);
#3909=VERTEX_POINT('',#11909);
#3910=VERTEX_POINT('',#11911);
#3911=VERTEX_POINT('',#11915);
#3912=VERTEX_POINT('',#11917);
#3913=VERTEX_POINT('',#11921);
#3914=VERTEX_POINT('',#11923);
#3915=VERTEX_POINT('',#11927);
#3916=VERTEX_POINT('',#11929);
#3917=VERTEX_POINT('',#11933);
#3918=VERTEX_POINT('',#11935);
#3919=VERTEX_POINT('',#11939);
#3920=VERTEX_POINT('',#11941);
#3921=VERTEX_POINT('',#11945);
#3922=VERTEX_POINT('',#11947);
#3923=VERTEX_POINT('',#11951);
#3924=VERTEX_POINT('',#11953);
#3925=VERTEX_POINT('',#11957);
#3926=VERTEX_POINT('',#11958);
#3927=VERTEX_POINT('',#11960);
#3928=VERTEX_POINT('',#11962);
#3929=VERTEX_POINT('',#11966);
#3930=VERTEX_POINT('',#11968);
#3931=VERTEX_POINT('',#11972);
#3932=VERTEX_POINT('',#11974);
#3933=VERTEX_POINT('',#11978);
#3934=VERTEX_POINT('',#11980);
#3935=VERTEX_POINT('',#11984);
#3936=VERTEX_POINT('',#11986);
#3937=VERTEX_POINT('',#11990);
#3938=VERTEX_POINT('',#11992);
#3939=VERTEX_POINT('',#11996);
#3940=VERTEX_POINT('',#11998);
#3941=VERTEX_POINT('',#12002);
#3942=VERTEX_POINT('',#12004);
#3943=VERTEX_POINT('',#12008);
#3944=VERTEX_POINT('',#12010);
#3945=VERTEX_POINT('',#12014);
#3946=VERTEX_POINT('',#12016);
#3947=VERTEX_POINT('',#12020);
#3948=VERTEX_POINT('',#12022);
#3949=VERTEX_POINT('',#12026);
#3950=VERTEX_POINT('',#12028);
#3951=VERTEX_POINT('',#12035);
#3952=VERTEX_POINT('',#12037);
#3953=VERTEX_POINT('',#12044);
#3954=VERTEX_POINT('',#12046);
#3955=VERTEX_POINT('',#12059);
#3956=VERTEX_POINT('',#12062);
#3957=VERTEX_POINT('',#12066);
#3958=VERTEX_POINT('',#12070);
#3959=VERTEX_POINT('',#12074);
#3960=VERTEX_POINT('',#12077);
#3961=VERTEX_POINT('',#12081);
#3962=VERTEX_POINT('',#12085);
#3963=VERTEX_POINT('',#12090);
#3964=VERTEX_POINT('',#12091);
#3965=VERTEX_POINT('',#12093);
#3966=VERTEX_POINT('',#12095);
#3967=VERTEX_POINT('',#12099);
#3968=VERTEX_POINT('',#12101);
#3969=VERTEX_POINT('',#12105);
#3970=VERTEX_POINT('',#12107);
#3971=VERTEX_POINT('',#12111);
#3972=VERTEX_POINT('',#12113);
#3973=VERTEX_POINT('',#12117);
#3974=VERTEX_POINT('',#12119);
#3975=VERTEX_POINT('',#12129);
#3976=VERTEX_POINT('',#12131);
#3977=VERTEX_POINT('',#12135);
#3978=VERTEX_POINT('',#12138);
#3979=VERTEX_POINT('',#12140);
#3980=VERTEX_POINT('',#12144);
#3981=VERTEX_POINT('',#12147);
#3982=VERTEX_POINT('',#12149);
#3983=VERTEX_POINT('',#12153);
#3984=VERTEX_POINT('',#12156);
#3985=VERTEX_POINT('',#12158);
#3986=VERTEX_POINT('',#12162);
#3987=VERTEX_POINT('',#12165);
#3988=VERTEX_POINT('',#12169);
#3989=VERTEX_POINT('',#12173);
#3990=VERTEX_POINT('',#12177);
#3991=VERTEX_POINT('',#12181);
#3992=VERTEX_POINT('',#12182);
#3993=VERTEX_POINT('',#12184);
#3994=VERTEX_POINT('',#12186);
#3995=VERTEX_POINT('',#12190);
#3996=VERTEX_POINT('',#12192);
#3997=VERTEX_POINT('',#12196);
#3998=VERTEX_POINT('',#12198);
#3999=VERTEX_POINT('',#12202);
#4000=VERTEX_POINT('',#12204);
#4001=VERTEX_POINT('',#12208);
#4002=VERTEX_POINT('',#12210);
#4003=VERTEX_POINT('',#12214);
#4004=VERTEX_POINT('',#12216);
#4005=VERTEX_POINT('',#12220);
#4006=VERTEX_POINT('',#12222);
#4007=VERTEX_POINT('',#12226);
#4008=VERTEX_POINT('',#12228);
#4009=VERTEX_POINT('',#12232);
#4010=VERTEX_POINT('',#12234);
#4011=VERTEX_POINT('',#12238);
#4012=VERTEX_POINT('',#12240);
#4013=VERTEX_POINT('',#12244);
#4014=VERTEX_POINT('',#12246);
#4015=VERTEX_POINT('',#12256);
#4016=VERTEX_POINT('',#12257);
#4017=VERTEX_POINT('',#12259);
#4018=VERTEX_POINT('',#12261);
#4019=VERTEX_POINT('',#12265);
#4020=VERTEX_POINT('',#12267);
#4021=VERTEX_POINT('',#12271);
#4022=VERTEX_POINT('',#12273);
#4023=VERTEX_POINT('',#12276);
#4024=VERTEX_POINT('',#12279);
#4025=VERTEX_POINT('',#12281);
#4026=VERTEX_POINT('',#12283);
#4027=VERTEX_POINT('',#12285);
#4028=VERTEX_POINT('',#12287);
#4029=VERTEX_POINT('',#12289);
#4030=VERTEX_POINT('',#12293);
#4031=VERTEX_POINT('',#12297);
#4032=VERTEX_POINT('',#12301);
#4033=VERTEX_POINT('',#12303);
#4034=VERTEX_POINT('',#12305);
#4035=VERTEX_POINT('',#12307);
#4036=VERTEX_POINT('',#12313);
#4037=VERTEX_POINT('',#12315);
#4038=VERTEX_POINT('',#12319);
#4039=VERTEX_POINT('',#12322);
#4040=VERTEX_POINT('',#12324);
#4041=VERTEX_POINT('',#12336);
#4042=VERTEX_POINT('',#12338);
#4043=VERTEX_POINT('',#12342);
#4044=VERTEX_POINT('',#12346);
#4045=VERTEX_POINT('',#12349);
#4046=VERTEX_POINT('',#12355);
#4047=VERTEX_POINT('',#12356);
#4048=VERTEX_POINT('',#12358);
#4049=VERTEX_POINT('',#12360);
#4050=VERTEX_POINT('',#12364);
#4051=VERTEX_POINT('',#12366);
#4052=VERTEX_POINT('',#12370);
#4053=VERTEX_POINT('',#12372);
#4054=VERTEX_POINT('',#12376);
#4055=VERTEX_POINT('',#12378);
#4056=VERTEX_POINT('',#12382);
#4057=VERTEX_POINT('',#12384);
#4058=VERTEX_POINT('',#12393);
#4059=VERTEX_POINT('',#12395);
#4060=VERTEX_POINT('',#12398);
#4061=VERTEX_POINT('',#12403);
#4062=VERTEX_POINT('',#12406);
#4063=VERTEX_POINT('',#12410);
#4064=VERTEX_POINT('',#12414);
#4065=VERTEX_POINT('',#12418);
#4066=VERTEX_POINT('',#12421);
#4067=VERTEX_POINT('',#12429);
#4068=VERTEX_POINT('',#12431);
#4069=VERTEX_POINT('',#12435);
#4070=VERTEX_POINT('',#12437);
#4071=VERTEX_POINT('',#12441);
#4072=VERTEX_POINT('',#12443);
#4073=VERTEX_POINT('',#12447);
#4074=VERTEX_POINT('',#12449);
#4075=VERTEX_POINT('',#12453);
#4076=VERTEX_POINT('',#12455);
#4077=VERTEX_POINT('',#12459);
#4078=VERTEX_POINT('',#12461);
#4079=VERTEX_POINT('',#12465);
#4080=VERTEX_POINT('',#12466);
#4081=VERTEX_POINT('',#12468);
#4082=VERTEX_POINT('',#12470);
#4083=VERTEX_POINT('',#12474);
#4084=VERTEX_POINT('',#12475);
#4085=VERTEX_POINT('',#12477);
#4086=VERTEX_POINT('',#12479);
#4087=VERTEX_POINT('',#12486);
#4088=VERTEX_POINT('',#12488);
#4089=VERTEX_POINT('',#12490);
#4090=VERTEX_POINT('',#12492);
#4091=VERTEX_POINT('',#12496);
#4092=VERTEX_POINT('',#12500);
#4093=VERTEX_POINT('',#12502);
#4094=VERTEX_POINT('',#12508);
#4095=VERTEX_POINT('',#12516);
#4096=VERTEX_POINT('',#12518);
#4097=VERTEX_POINT('',#12523);
#4098=VERTEX_POINT('',#12525);
#4099=VERTEX_POINT('',#12530);
#4100=VERTEX_POINT('',#12532);
#4101=VERTEX_POINT('',#12534);
#4102=VERTEX_POINT('',#12541);
#4103=VERTEX_POINT('',#12545);
#4104=VERTEX_POINT('',#12547);
#4105=VERTEX_POINT('',#12549);
#4106=VERTEX_POINT('',#12556);
#4107=VERTEX_POINT('',#12564);
#4108=VERTEX_POINT('',#12565);
#4109=VERTEX_POINT('',#12569);
#4110=VERTEX_POINT('',#12571);
#4111=VERTEX_POINT('',#12573);
#4112=VERTEX_POINT('',#12576);
#4113=VERTEX_POINT('',#12580);
#4114=VERTEX_POINT('',#12581);
#4115=VERTEX_POINT('',#12585);
#4116=VERTEX_POINT('',#12587);
#4117=VERTEX_POINT('',#12589);
#4118=VERTEX_POINT('',#12592);
#4119=VERTEX_POINT('',#12596);
#4120=VERTEX_POINT('',#12597);
#4121=VERTEX_POINT('',#12601);
#4122=VERTEX_POINT('',#12603);
#4123=VERTEX_POINT('',#12605);
#4124=VERTEX_POINT('',#12608);
#4125=VERTEX_POINT('',#12612);
#4126=VERTEX_POINT('',#12613);
#4127=VERTEX_POINT('',#12617);
#4128=VERTEX_POINT('',#12619);
#4129=VERTEX_POINT('',#12621);
#4130=VERTEX_POINT('',#12624);
#4131=VERTEX_POINT('',#12629);
#4132=VERTEX_POINT('',#12631);
#4133=VERTEX_POINT('',#12633);
#4134=VERTEX_POINT('',#12635);
#4135=VERTEX_POINT('',#12640);
#4136=VERTEX_POINT('',#12642);
#4137=VERTEX_POINT('',#12644);
#4138=VERTEX_POINT('',#12646);
#4139=VERTEX_POINT('',#12650);
#4140=VERTEX_POINT('',#12652);
#4141=VERTEX_POINT('',#12654);
#4142=VERTEX_POINT('',#12656);
#4143=VERTEX_POINT('',#12659);
#4144=VERTEX_POINT('',#12661);
#4145=VERTEX_POINT('',#12663);
#4146=VERTEX_POINT('',#12665);
#4147=VERTEX_POINT('',#12669);
#4148=VERTEX_POINT('',#12673);
#4149=VERTEX_POINT('',#12677);
#4150=VERTEX_POINT('',#12681);
#4151=VERTEX_POINT('',#12687);
#4152=VERTEX_POINT('',#12691);
#4153=VERTEX_POINT('',#12695);
#4154=VERTEX_POINT('',#12699);
#4155=VERTEX_POINT('',#12707);
#4156=VERTEX_POINT('',#12708);
#4157=VERTEX_POINT('',#12710);
#4158=VERTEX_POINT('',#12712);
#4159=VERTEX_POINT('',#12716);
#4160=VERTEX_POINT('',#12718);
#4161=VERTEX_POINT('',#12722);
#4162=VERTEX_POINT('',#12724);
#4163=VERTEX_POINT('',#12728);
#4164=VERTEX_POINT('',#12730);
#4165=VERTEX_POINT('',#12734);
#4166=VERTEX_POINT('',#12736);
#4167=VERTEX_POINT('',#12740);
#4168=VERTEX_POINT('',#12742);
#4169=VERTEX_POINT('',#12746);
#4170=VERTEX_POINT('',#12748);
#4171=VERTEX_POINT('',#12758);
#4172=VERTEX_POINT('',#12759);
#4173=VERTEX_POINT('',#12761);
#4174=VERTEX_POINT('',#12763);
#4175=VERTEX_POINT('',#12767);
#4176=VERTEX_POINT('',#12769);
#4177=VERTEX_POINT('',#12773);
#4178=VERTEX_POINT('',#12775);
#4179=VERTEX_POINT('',#12779);
#4180=VERTEX_POINT('',#12781);
#4181=VERTEX_POINT('',#12785);
#4182=VERTEX_POINT('',#12787);
#4183=VERTEX_POINT('',#12791);
#4184=VERTEX_POINT('',#12793);
#4185=VERTEX_POINT('',#12797);
#4186=VERTEX_POINT('',#12799);
#4187=VERTEX_POINT('',#12812);
#4188=VERTEX_POINT('',#12813);
#4189=VERTEX_POINT('',#12815);
#4190=VERTEX_POINT('',#12817);
#4191=VERTEX_POINT('',#12821);
#4192=VERTEX_POINT('',#12823);
#4193=VERTEX_POINT('',#12827);
#4194=VERTEX_POINT('',#12829);
#4195=VERTEX_POINT('',#12833);
#4196=VERTEX_POINT('',#12835);
#4197=VERTEX_POINT('',#12839);
#4198=VERTEX_POINT('',#12841);
#4199=VERTEX_POINT('',#12850);
#4200=VERTEX_POINT('',#12853);
#4201=VERTEX_POINT('',#12856);
#4202=VERTEX_POINT('',#12860);
#4203=VERTEX_POINT('',#12864);
#4204=VERTEX_POINT('',#12868);
#4205=VERTEX_POINT('',#12871);
#4206=VERTEX_POINT('',#12878);
#4207=VERTEX_POINT('',#12881);
#4208=VERTEX_POINT('',#12885);
#4209=VERTEX_POINT('',#12889);
#4210=VERTEX_POINT('',#12893);
#4211=VERTEX_POINT('',#12896);
#4212=VERTEX_POINT('',#12900);
#4213=VERTEX_POINT('',#12904);
#4214=VERTEX_POINT('',#12909);
#4215=VERTEX_POINT('',#12910);
#4216=VERTEX_POINT('',#12912);
#4217=VERTEX_POINT('',#12914);
#4218=VERTEX_POINT('',#12918);
#4219=VERTEX_POINT('',#12920);
#4220=VERTEX_POINT('',#12924);
#4221=VERTEX_POINT('',#12926);
#4222=VERTEX_POINT('',#12930);
#4223=VERTEX_POINT('',#12932);
#4224=VERTEX_POINT('',#12936);
#4225=VERTEX_POINT('',#12938);
#4226=EDGE_CURVE('',#3593,#3593,#3414,.T.);
#4227=EDGE_CURVE('',#3593,#3594,#1860,.T.);
#4228=EDGE_CURVE('',#3594,#3594,#3415,.T.);
#4229=EDGE_CURVE('',#3595,#3595,#3416,.T.);
#4230=EDGE_CURVE('',#3595,#3596,#1861,.T.);
#4231=EDGE_CURVE('',#3596,#3596,#3417,.T.);
#4232=EDGE_CURVE('',#3597,#3597,#3418,.T.);
#4233=EDGE_CURVE('',#3597,#3598,#1862,.T.);
#4234=EDGE_CURVE('',#3598,#3598,#3419,.T.);
#4235=EDGE_CURVE('',#3599,#3599,#3420,.T.);
#4236=EDGE_CURVE('',#3599,#3600,#1863,.T.);
#4237=EDGE_CURVE('',#3600,#3600,#3421,.T.);
#4238=EDGE_CURVE('',#3601,#3602,#1864,.T.);
#4239=EDGE_CURVE('',#3602,#3603,#1865,.T.);
#4240=EDGE_CURVE('',#3604,#3603,#1866,.T.);
#4241=EDGE_CURVE('',#3601,#3604,#1867,.T.);
#4242=EDGE_CURVE('',#3605,#3601,#1868,.T.);
#4243=EDGE_CURVE('',#3606,#3604,#1869,.T.);
#4244=EDGE_CURVE('',#3605,#3606,#1870,.T.);
#4245=EDGE_CURVE('',#3607,#3605,#1871,.T.);
#4246=EDGE_CURVE('',#3608,#3606,#1872,.T.);
#4247=EDGE_CURVE('',#3607,#3608,#1873,.T.);
#4248=EDGE_CURVE('',#3602,#3607,#1874,.T.);
#4249=EDGE_CURVE('',#3603,#3608,#1875,.T.);
#4250=EDGE_CURVE('',#3609,#3609,#3422,.T.);
#4251=EDGE_CURVE('',#3609,#3610,#1876,.T.);
#4252=EDGE_CURVE('',#3610,#3610,#3423,.T.);
#4253=EDGE_CURVE('',#3611,#3611,#3424,.T.);
#4254=EDGE_CURVE('',#3611,#3612,#1877,.T.);
#4255=EDGE_CURVE('',#3612,#3612,#3425,.T.);
#4256=EDGE_CURVE('',#3613,#3613,#3426,.T.);
#4257=EDGE_CURVE('',#3613,#3614,#1878,.T.);
#4258=EDGE_CURVE('',#3614,#3614,#3427,.T.);
#4259=EDGE_CURVE('',#3615,#3615,#3428,.T.);
#4260=EDGE_CURVE('',#3615,#3616,#1879,.T.);
#4261=EDGE_CURVE('',#3616,#3616,#3429,.T.);
#4262=EDGE_CURVE('',#3617,#3618,#1880,.T.);
#4263=EDGE_CURVE('',#3619,#3617,#1881,.T.);
#4264=EDGE_CURVE('',#3620,#3619,#1882,.T.);
#4265=EDGE_CURVE('',#3620,#3618,#1883,.T.);
#4266=EDGE_CURVE('',#3618,#3621,#1884,.T.);
#4267=EDGE_CURVE('',#3622,#3620,#1885,.T.);
#4268=EDGE_CURVE('',#3622,#3621,#1886,.T.);
#4269=EDGE_CURVE('',#3621,#3623,#1887,.T.);
#4270=EDGE_CURVE('',#3624,#3622,#1888,.T.);
#4271=EDGE_CURVE('',#3624,#3623,#1889,.T.);
#4272=EDGE_CURVE('',#3623,#3617,#1890,.T.);
#4273=EDGE_CURVE('',#3619,#3624,#1891,.T.);
#4274=EDGE_CURVE('',#3625,#3626,#1892,.T.);
#4275=EDGE_CURVE('',#3626,#3627,#1893,.T.);
#4276=EDGE_CURVE('',#3628,#3627,#1894,.T.);
#4277=EDGE_CURVE('',#3625,#3628,#1895,.T.);
#4278=EDGE_CURVE('',#3629,#3625,#1896,.T.);
#4279=EDGE_CURVE('',#3630,#3628,#1897,.T.);
#4280=EDGE_CURVE('',#3629,#3630,#1898,.T.);
#4281=EDGE_CURVE('',#3631,#3629,#1899,.T.);
#4282=EDGE_CURVE('',#3632,#3630,#1900,.T.);
#4283=EDGE_CURVE('',#3631,#3632,#1901,.T.);
#4284=EDGE_CURVE('',#3626,#3631,#1902,.T.);
#4285=EDGE_CURVE('',#3627,#3632,#1903,.T.);
#4286=EDGE_CURVE('',#3633,#3634,#1904,.T.);
#4287=EDGE_CURVE('',#3634,#3635,#1905,.T.);
#4288=EDGE_CURVE('',#3636,#3635,#1906,.T.);
#4289=EDGE_CURVE('',#3633,#3636,#1907,.T.);
#4290=EDGE_CURVE('',#3637,#3633,#1908,.T.);
#4291=EDGE_CURVE('',#3638,#3636,#1909,.T.);
#4292=EDGE_CURVE('',#3637,#3638,#1910,.T.);
#4293=EDGE_CURVE('',#3639,#3637,#1911,.T.);
#4294=EDGE_CURVE('',#3640,#3638,#1912,.T.);
#4295=EDGE_CURVE('',#3639,#3640,#1913,.T.);
#4296=EDGE_CURVE('',#3634,#3639,#1914,.T.);
#4297=EDGE_CURVE('',#3635,#3640,#1915,.T.);
#4298=EDGE_CURVE('',#3641,#3642,#1916,.T.);
#4299=EDGE_CURVE('',#3642,#3643,#1917,.T.);
#4300=EDGE_CURVE('',#3644,#3643,#1918,.T.);
#4301=EDGE_CURVE('',#3641,#3644,#1919,.T.);
#4302=EDGE_CURVE('',#3645,#3641,#1920,.T.);
#4303=EDGE_CURVE('',#3646,#3644,#1921,.T.);
#4304=EDGE_CURVE('',#3645,#3646,#1922,.T.);
#4305=EDGE_CURVE('',#3647,#3645,#1923,.T.);
#4306=EDGE_CURVE('',#3648,#3646,#1924,.T.);
#4307=EDGE_CURVE('',#3647,#3648,#1925,.T.);
#4308=EDGE_CURVE('',#3642,#3647,#1926,.T.);
#4309=EDGE_CURVE('',#3643,#3648,#1927,.T.);
#4310=EDGE_CURVE('',#3649,#3650,#1928,.T.);
#4311=EDGE_CURVE('',#3649,#3651,#1929,.T.);
#4312=EDGE_CURVE('',#3652,#3651,#1930,.T.);
#4313=EDGE_CURVE('',#3650,#3652,#1931,.T.);
#4314=EDGE_CURVE('',#3650,#3653,#1932,.T.);
#4315=EDGE_CURVE('',#3654,#3652,#1933,.T.);
#4316=EDGE_CURVE('',#3653,#3654,#1934,.T.);
#4317=EDGE_CURVE('',#3653,#3655,#1935,.T.);
#4318=EDGE_CURVE('',#3656,#3654,#1936,.T.);
#4319=EDGE_CURVE('',#3655,#3656,#1937,.T.);
#4320=EDGE_CURVE('',#3655,#3649,#1938,.T.);
#4321=EDGE_CURVE('',#3651,#3656,#1939,.T.);
#4322=EDGE_CURVE('',#3657,#3657,#3430,.T.);
#4323=EDGE_CURVE('',#3657,#3658,#1940,.T.);
#4324=EDGE_CURVE('',#3658,#3658,#3431,.T.);
#4325=EDGE_CURVE('',#3659,#3659,#3432,.T.);
#4326=EDGE_CURVE('',#3659,#3660,#1941,.T.);
#4327=EDGE_CURVE('',#3660,#3660,#3433,.T.);
#4328=EDGE_CURVE('',#3661,#3662,#1942,.T.);
#4329=EDGE_CURVE('',#3661,#3663,#1943,.T.);
#4330=EDGE_CURVE('',#3664,#3663,#1944,.T.);
#4331=EDGE_CURVE('',#3662,#3664,#1945,.T.);
#4332=EDGE_CURVE('',#3662,#3665,#1946,.T.);
#4333=EDGE_CURVE('',#3666,#3664,#1947,.T.);
#4334=EDGE_CURVE('',#3665,#3666,#1948,.T.);
#4335=EDGE_CURVE('',#3665,#3667,#1949,.T.);
#4336=EDGE_CURVE('',#3668,#3666,#1950,.T.);
#4337=EDGE_CURVE('',#3667,#3668,#1951,.T.);
#4338=EDGE_CURVE('',#3667,#3661,#1952,.T.);
#4339=EDGE_CURVE('',#3663,#3668,#1953,.T.);
#4340=EDGE_CURVE('',#3669,#3669,#3434,.T.);
#4341=EDGE_CURVE('',#3669,#3670,#1954,.T.);
#4342=EDGE_CURVE('',#3670,#3670,#3435,.T.);
#4343=EDGE_CURVE('',#3671,#3671,#3436,.T.);
#4344=EDGE_CURVE('',#3671,#3672,#1955,.T.);
#4345=EDGE_CURVE('',#3672,#3672,#3437,.T.);
#4346=EDGE_CURVE('',#3673,#3674,#1956,.T.);
#4347=EDGE_CURVE('',#3673,#3675,#1957,.T.);
#4348=EDGE_CURVE('',#3676,#3675,#1958,.T.);
#4349=EDGE_CURVE('',#3674,#3676,#1959,.T.);
#4350=EDGE_CURVE('',#3674,#3677,#1960,.T.);
#4351=EDGE_CURVE('',#3678,#3676,#1961,.T.);
#4352=EDGE_CURVE('',#3677,#3678,#1962,.T.);
#4353=EDGE_CURVE('',#3677,#3679,#1963,.T.);
#4354=EDGE_CURVE('',#3680,#3678,#1964,.T.);
#4355=EDGE_CURVE('',#3679,#3680,#1965,.T.);
#4356=EDGE_CURVE('',#3679,#3673,#1966,.T.);
#4357=EDGE_CURVE('',#3675,#3680,#1967,.T.);
#4358=EDGE_CURVE('',#3681,#3681,#3438,.T.);
#4359=EDGE_CURVE('',#3681,#3682,#1968,.T.);
#4360=EDGE_CURVE('',#3682,#3682,#3439,.T.);
#4361=EDGE_CURVE('',#3683,#3683,#3440,.T.);
#4362=EDGE_CURVE('',#3683,#3684,#1969,.T.);
#4363=EDGE_CURVE('',#3684,#3684,#3441,.T.);
#4364=EDGE_CURVE('',#3685,#3685,#3442,.T.);
#4365=EDGE_CURVE('',#3686,#3686,#3443,.T.);
#4366=EDGE_CURVE('',#3686,#3685,#1970,.T.);
#4367=EDGE_CURVE('',#3687,#3688,#1971,.T.);
#4368=EDGE_CURVE('',#3688,#3689,#1972,.T.);
#4369=EDGE_CURVE('',#3690,#3689,#1973,.T.);
#4370=EDGE_CURVE('',#3687,#3690,#1974,.T.);
#4371=EDGE_CURVE('',#3691,#3687,#1975,.T.);
#4372=EDGE_CURVE('',#3692,#3690,#1976,.T.);
#4373=EDGE_CURVE('',#3691,#3692,#1977,.T.);
#4374=EDGE_CURVE('',#3693,#3691,#1978,.T.);
#4375=EDGE_CURVE('',#3694,#3692,#1979,.T.);
#4376=EDGE_CURVE('',#3693,#3694,#1980,.T.);
#4377=EDGE_CURVE('',#3688,#3693,#1981,.T.);
#4378=EDGE_CURVE('',#3689,#3694,#1982,.T.);
#4379=EDGE_CURVE('',#3695,#3695,#3444,.T.);
#4380=EDGE_CURVE('',#3695,#3696,#1983,.T.);
#4381=EDGE_CURVE('',#3696,#3696,#3445,.T.);
#4382=EDGE_CURVE('',#3697,#3697,#3446,.T.);
#4383=EDGE_CURVE('',#3697,#3698,#1984,.T.);
#4384=EDGE_CURVE('',#3698,#3698,#3447,.T.);
#4385=EDGE_CURVE('',#3699,#3699,#3448,.T.);
#4386=EDGE_CURVE('',#3699,#3700,#1985,.T.);
#4387=EDGE_CURVE('',#3700,#3700,#3449,.T.);
#4388=EDGE_CURVE('',#3701,#3702,#1986,.T.);
#4389=EDGE_CURVE('',#3702,#3703,#1987,.T.);
#4390=EDGE_CURVE('',#3704,#3703,#1988,.T.);
#4391=EDGE_CURVE('',#3701,#3704,#1989,.T.);
#4392=EDGE_CURVE('',#3705,#3701,#1990,.T.);
#4393=EDGE_CURVE('',#3706,#3704,#1991,.T.);
#4394=EDGE_CURVE('',#3705,#3706,#1992,.T.);
#4395=EDGE_CURVE('',#3707,#3705,#1993,.T.);
#4396=EDGE_CURVE('',#3708,#3706,#1994,.T.);
#4397=EDGE_CURVE('',#3707,#3708,#1995,.T.);
#4398=EDGE_CURVE('',#3702,#3707,#1996,.T.);
#4399=EDGE_CURVE('',#3703,#3708,#1997,.T.);
#4400=EDGE_CURVE('',#3709,#3709,#3450,.T.);
#4401=EDGE_CURVE('',#3709,#3710,#1998,.T.);
#4402=EDGE_CURVE('',#3710,#3710,#3451,.T.);
#4403=EDGE_CURVE('',#3711,#3711,#3452,.T.);
#4404=EDGE_CURVE('',#3711,#3712,#1999,.T.);
#4405=EDGE_CURVE('',#3712,#3712,#3453,.T.);
#4406=EDGE_CURVE('',#3713,#3713,#3454,.T.);
#4407=EDGE_CURVE('',#3714,#3714,#3455,.T.);
#4408=EDGE_CURVE('',#3714,#3713,#2000,.T.);
#4409=EDGE_CURVE('',#3715,#3716,#2001,.T.);
#4410=EDGE_CURVE('',#3716,#3717,#2002,.T.);
#4411=EDGE_CURVE('',#3718,#3717,#2003,.T.);
#4412=EDGE_CURVE('',#3715,#3718,#2004,.T.);
#4413=EDGE_CURVE('',#3719,#3715,#2005,.T.);
#4414=EDGE_CURVE('',#3720,#3718,#2006,.T.);
#4415=EDGE_CURVE('',#3719,#3720,#2007,.T.);
#4416=EDGE_CURVE('',#3721,#3719,#2008,.T.);
#4417=EDGE_CURVE('',#3722,#3720,#2009,.T.);
#4418=EDGE_CURVE('',#3721,#3722,#2010,.T.);
#4419=EDGE_CURVE('',#3716,#3721,#2011,.T.);
#4420=EDGE_CURVE('',#3717,#3722,#2012,.T.);
#4421=EDGE_CURVE('',#3723,#3723,#3456,.T.);
#4422=EDGE_CURVE('',#3723,#3724,#2013,.T.);
#4423=EDGE_CURVE('',#3724,#3724,#3457,.T.);
#4424=EDGE_CURVE('',#3725,#3725,#3458,.T.);
#4425=EDGE_CURVE('',#3725,#3726,#2014,.T.);
#4426=EDGE_CURVE('',#3726,#3726,#3459,.T.);
#4427=EDGE_CURVE('',#3727,#3727,#3460,.T.);
#4428=EDGE_CURVE('',#3727,#3728,#2015,.T.);
#4429=EDGE_CURVE('',#3728,#3728,#3461,.T.);
#4430=EDGE_CURVE('',#3729,#3730,#2016,.T.);
#4431=EDGE_CURVE('',#3730,#3731,#2017,.T.);
#4432=EDGE_CURVE('',#3732,#3731,#2018,.T.);
#4433=EDGE_CURVE('',#3729,#3732,#2019,.T.);
#4434=EDGE_CURVE('',#3733,#3729,#2020,.T.);
#4435=EDGE_CURVE('',#3734,#3732,#2021,.T.);
#4436=EDGE_CURVE('',#3733,#3734,#2022,.T.);
#4437=EDGE_CURVE('',#3735,#3733,#2023,.T.);
#4438=EDGE_CURVE('',#3736,#3734,#2024,.T.);
#4439=EDGE_CURVE('',#3735,#3736,#2025,.T.);
#4440=EDGE_CURVE('',#3730,#3735,#2026,.T.);
#4441=EDGE_CURVE('',#3731,#3736,#2027,.T.);
#4442=EDGE_CURVE('',#3737,#3738,#2028,.T.);
#4443=EDGE_CURVE('',#3739,#3737,#2029,.T.);
#4444=EDGE_CURVE('',#3740,#3739,#2030,.T.);
#4445=EDGE_CURVE('',#3740,#3738,#2031,.T.);
#4446=EDGE_CURVE('',#3738,#3741,#2032,.T.);
#4447=EDGE_CURVE('',#3742,#3740,#2033,.T.);
#4448=EDGE_CURVE('',#3742,#3741,#2034,.T.);
#4449=EDGE_CURVE('',#3741,#3743,#2035,.T.);
#4450=EDGE_CURVE('',#3744,#3742,#2036,.T.);
#4451=EDGE_CURVE('',#3744,#3743,#2037,.T.);
#4452=EDGE_CURVE('',#3743,#3737,#2038,.T.);
#4453=EDGE_CURVE('',#3739,#3744,#2039,.T.);
#4454=EDGE_CURVE('',#3745,#3746,#2040,.T.);
#4455=EDGE_CURVE('',#3746,#3747,#2041,.T.);
#4456=EDGE_CURVE('',#3748,#3747,#2042,.T.);
#4457=EDGE_CURVE('',#3745,#3748,#2043,.T.);
#4458=EDGE_CURVE('',#3749,#3745,#2044,.T.);
#4459=EDGE_CURVE('',#3750,#3748,#2045,.T.);
#4460=EDGE_CURVE('',#3749,#3750,#2046,.T.);
#4461=EDGE_CURVE('',#3751,#3749,#2047,.T.);
#4462=EDGE_CURVE('',#3752,#3750,#2048,.T.);
#4463=EDGE_CURVE('',#3751,#3752,#2049,.T.);
#4464=EDGE_CURVE('',#3746,#3751,#2050,.T.);
#4465=EDGE_CURVE('',#3747,#3752,#2051,.T.);
#4466=EDGE_CURVE('',#3753,#3754,#2052,.T.);
#4467=EDGE_CURVE('',#3755,#3753,#2053,.T.);
#4468=EDGE_CURVE('',#3756,#3755,#2054,.T.);
#4469=EDGE_CURVE('',#3756,#3754,#2055,.T.);
#4470=EDGE_CURVE('',#3754,#3757,#2056,.T.);
#4471=EDGE_CURVE('',#3758,#3756,#2057,.T.);
#4472=EDGE_CURVE('',#3758,#3757,#2058,.T.);
#4473=EDGE_CURVE('',#3757,#3759,#2059,.T.);
#4474=EDGE_CURVE('',#3760,#3758,#2060,.T.);
#4475=EDGE_CURVE('',#3760,#3759,#2061,.T.);
#4476=EDGE_CURVE('',#3759,#3753,#2062,.T.);
#4477=EDGE_CURVE('',#3755,#3760,#2063,.T.);
#4478=EDGE_CURVE('',#3761,#3762,#2064,.T.);
#4479=EDGE_CURVE('',#3762,#3763,#2065,.T.);
#4480=EDGE_CURVE('',#3764,#3763,#2066,.T.);
#4481=EDGE_CURVE('',#3761,#3764,#2067,.T.);
#4482=EDGE_CURVE('',#3765,#3761,#2068,.T.);
#4483=EDGE_CURVE('',#3766,#3764,#2069,.T.);
#4484=EDGE_CURVE('',#3765,#3766,#2070,.T.);
#4485=EDGE_CURVE('',#3767,#3765,#2071,.T.);
#4486=EDGE_CURVE('',#3768,#3766,#2072,.T.);
#4487=EDGE_CURVE('',#3767,#3768,#2073,.T.);
#4488=EDGE_CURVE('',#3762,#3767,#2074,.T.);
#4489=EDGE_CURVE('',#3763,#3768,#2075,.T.);
#4490=EDGE_CURVE('',#3769,#3769,#3462,.T.);
#4491=EDGE_CURVE('',#3769,#3770,#2076,.T.);
#4492=EDGE_CURVE('',#3770,#3770,#3463,.T.);
#4493=EDGE_CURVE('',#3771,#3771,#3464,.T.);
#4494=EDGE_CURVE('',#3771,#3772,#2077,.T.);
#4495=EDGE_CURVE('',#3772,#3772,#3465,.T.);
#4496=EDGE_CURVE('',#3773,#3773,#3466,.T.);
#4497=EDGE_CURVE('',#3773,#3774,#2078,.T.);
#4498=EDGE_CURVE('',#3774,#3774,#3467,.T.);
#4499=EDGE_CURVE('',#3775,#3775,#3468,.T.);
#4500=EDGE_CURVE('',#3775,#3776,#2079,.T.);
#4501=EDGE_CURVE('',#3776,#3776,#3469,.T.);
#4502=EDGE_CURVE('',#3777,#3777,#3470,.T.);
#4503=EDGE_CURVE('',#3777,#3778,#2080,.T.);
#4504=EDGE_CURVE('',#3778,#3778,#3471,.T.);
#4505=EDGE_CURVE('',#3779,#3779,#3472,.T.);
#4506=EDGE_CURVE('',#3779,#3780,#2081,.T.);
#4507=EDGE_CURVE('',#3780,#3780,#3473,.T.);
#4508=EDGE_CURVE('',#3781,#3781,#3474,.T.);
#4509=EDGE_CURVE('',#3781,#3782,#2082,.T.);
#4510=EDGE_CURVE('',#3782,#3782,#3475,.T.);
#4511=EDGE_CURVE('',#3783,#3783,#3476,.T.);
#4512=EDGE_CURVE('',#3783,#3784,#2083,.T.);
#4513=EDGE_CURVE('',#3784,#3784,#3477,.T.);
#4514=EDGE_CURVE('',#3785,#3786,#2084,.T.);
#4515=EDGE_CURVE('',#3786,#3787,#2085,.T.);
#4516=EDGE_CURVE('',#3788,#3787,#2086,.T.);
#4517=EDGE_CURVE('',#3785,#3788,#2087,.T.);
#4518=EDGE_CURVE('',#3789,#3785,#2088,.T.);
#4519=EDGE_CURVE('',#3790,#3788,#2089,.T.);
#4520=EDGE_CURVE('',#3789,#3790,#2090,.T.);
#4521=EDGE_CURVE('',#3791,#3789,#2091,.T.);
#4522=EDGE_CURVE('',#3792,#3790,#2092,.T.);
#4523=EDGE_CURVE('',#3791,#3792,#2093,.T.);
#4524=EDGE_CURVE('',#3786,#3791,#2094,.T.);
#4525=EDGE_CURVE('',#3787,#3792,#2095,.T.);
#4526=EDGE_CURVE('',#3793,#3793,#3478,.T.);
#4527=EDGE_CURVE('',#3793,#3794,#2096,.T.);
#4528=EDGE_CURVE('',#3794,#3794,#3479,.T.);
#4529=EDGE_CURVE('',#3795,#3795,#3480,.T.);
#4530=EDGE_CURVE('',#3795,#3796,#2097,.T.);
#4531=EDGE_CURVE('',#3796,#3796,#3481,.T.);
#4532=EDGE_CURVE('',#3797,#3798,#2098,.T.);
#4533=EDGE_CURVE('',#3798,#3799,#2099,.T.);
#4534=EDGE_CURVE('',#3800,#3799,#2100,.T.);
#4535=EDGE_CURVE('',#3797,#3800,#2101,.T.);
#4536=EDGE_CURVE('',#3801,#3797,#2102,.T.);
#4537=EDGE_CURVE('',#3802,#3800,#2103,.T.);
#4538=EDGE_CURVE('',#3801,#3802,#2104,.T.);
#4539=EDGE_CURVE('',#3803,#3801,#2105,.T.);
#4540=EDGE_CURVE('',#3804,#3802,#2106,.T.);
#4541=EDGE_CURVE('',#3803,#3804,#2107,.T.);
#4542=EDGE_CURVE('',#3805,#3803,#2108,.T.);
#4543=EDGE_CURVE('',#3806,#3804,#2109,.T.);
#4544=EDGE_CURVE('',#3805,#3806,#2110,.T.);
#4545=EDGE_CURVE('',#3807,#3805,#2111,.T.);
#4546=EDGE_CURVE('',#3808,#3806,#2112,.T.);
#4547=EDGE_CURVE('',#3807,#3808,#2113,.T.);
#4548=EDGE_CURVE('',#3798,#3807,#2114,.T.);
#4549=EDGE_CURVE('',#3799,#3808,#2115,.T.);
#4550=EDGE_CURVE('',#3809,#3809,#3482,.T.);
#4551=EDGE_CURVE('',#3809,#3810,#2116,.T.);
#4552=EDGE_CURVE('',#3810,#3810,#3483,.T.);
#4553=EDGE_CURVE('',#3811,#3811,#3484,.T.);
#4554=EDGE_CURVE('',#3811,#3812,#2117,.T.);
#4555=EDGE_CURVE('',#3812,#3812,#3485,.T.);
#4556=EDGE_CURVE('',#3813,#3814,#2118,.T.);
#4557=EDGE_CURVE('',#3815,#3813,#2119,.T.);
#4558=EDGE_CURVE('',#3816,#3815,#2120,.T.);
#4559=EDGE_CURVE('',#3814,#3816,#2121,.T.);
#4560=EDGE_CURVE('',#3816,#3817,#2122,.T.);
#4561=EDGE_CURVE('',#3818,#3815,#2123,.T.);
#4562=EDGE_CURVE('',#3817,#3818,#2124,.T.);
#4563=EDGE_CURVE('',#3814,#3819,#2125,.T.);
#4564=EDGE_CURVE('',#3817,#3819,#2126,.T.);
#4565=EDGE_CURVE('',#3813,#3820,#2127,.T.);
#4566=EDGE_CURVE('',#3821,#3820,#2128,.T.);
#4567=EDGE_CURVE('',#3822,#3821,#2129,.T.);
#4568=EDGE_CURVE('',#3822,#3818,#2130,.T.);
#4569=EDGE_CURVE('',#3823,#3822,#2131,.T.);
#4570=EDGE_CURVE('',#3824,#3823,#2132,.T.);
#4571=EDGE_CURVE('',#3819,#3824,#2133,.T.);
#4572=EDGE_CURVE('',#3825,#3821,#2134,.T.);
#4573=EDGE_CURVE('',#3823,#3825,#2135,.T.);
#4574=EDGE_CURVE('',#3826,#3825,#2136,.T.);
#4575=EDGE_CURVE('',#3824,#3826,#2137,.T.);
#4576=EDGE_CURVE('',#3820,#3826,#2138,.T.);
#4577=EDGE_CURVE('',#3827,#3827,#3486,.T.);
#4578=EDGE_CURVE('',#3827,#3828,#2139,.T.);
#4579=EDGE_CURVE('',#3828,#3828,#3487,.T.);
#4580=EDGE_CURVE('',#3829,#3829,#3488,.T.);
#4581=EDGE_CURVE('',#3829,#3830,#2140,.T.);
#4582=EDGE_CURVE('',#3830,#3830,#3489,.T.);
#4583=EDGE_CURVE('',#3831,#3832,#2141,.T.);
#4584=EDGE_CURVE('',#3833,#3831,#2142,.T.);
#4585=EDGE_CURVE('',#3834,#3833,#2143,.T.);
#4586=EDGE_CURVE('',#3832,#3834,#2144,.T.);
#4587=EDGE_CURVE('',#3834,#3835,#2145,.T.);
#4588=EDGE_CURVE('',#3836,#3833,#2146,.T.);
#4589=EDGE_CURVE('',#3835,#3836,#2147,.T.);
#4590=EDGE_CURVE('',#3832,#3837,#2148,.T.);
#4591=EDGE_CURVE('',#3835,#3837,#2149,.T.);
#4592=EDGE_CURVE('',#3831,#3838,#2150,.T.);
#4593=EDGE_CURVE('',#3839,#3838,#2151,.T.);
#4594=EDGE_CURVE('',#3840,#3839,#2152,.T.);
#4595=EDGE_CURVE('',#3840,#3836,#2153,.T.);
#4596=EDGE_CURVE('',#3841,#3840,#2154,.T.);
#4597=EDGE_CURVE('',#3842,#3841,#2155,.T.);
#4598=EDGE_CURVE('',#3837,#3842,#2156,.T.);
#4599=EDGE_CURVE('',#3843,#3839,#2157,.T.);
#4600=EDGE_CURVE('',#3841,#3843,#2158,.T.);
#4601=EDGE_CURVE('',#3844,#3843,#2159,.T.);
#4602=EDGE_CURVE('',#3842,#3844,#2160,.T.);
#4603=EDGE_CURVE('',#3838,#3844,#2161,.T.);
#4604=EDGE_CURVE('',#3845,#3845,#3490,.T.);
#4605=EDGE_CURVE('',#3845,#3846,#2162,.T.);
#4606=EDGE_CURVE('',#3846,#3846,#3491,.T.);
#4607=EDGE_CURVE('',#3847,#3848,#2163,.T.);
#4608=EDGE_CURVE('',#3848,#3849,#2164,.T.);
#4609=EDGE_CURVE('',#3850,#3849,#2165,.T.);
#4610=EDGE_CURVE('',#3847,#3850,#2166,.T.);
#4611=EDGE_CURVE('',#3851,#3847,#2167,.T.);
#4612=EDGE_CURVE('',#3852,#3850,#2168,.T.);
#4613=EDGE_CURVE('',#3851,#3852,#2169,.T.);
#4614=EDGE_CURVE('',#3853,#3851,#2170,.T.);
#4615=EDGE_CURVE('',#3854,#3852,#2171,.T.);
#4616=EDGE_CURVE('',#3853,#3854,#2172,.T.);
#4617=EDGE_CURVE('',#3848,#3853,#2173,.T.);
#4618=EDGE_CURVE('',#3849,#3854,#2174,.T.);
#4619=EDGE_CURVE('',#3855,#3855,#3492,.T.);
#4620=EDGE_CURVE('',#3855,#3856,#2175,.T.);
#4621=EDGE_CURVE('',#3856,#3856,#3493,.T.);
#4622=EDGE_CURVE('',#3857,#3858,#2176,.T.);
#4623=EDGE_CURVE('',#3858,#3859,#2177,.T.);
#4624=EDGE_CURVE('',#3860,#3859,#2178,.T.);
#4625=EDGE_CURVE('',#3857,#3860,#2179,.T.);
#4626=EDGE_CURVE('',#3861,#3857,#2180,.T.);
#4627=EDGE_CURVE('',#3862,#3860,#2181,.T.);
#4628=EDGE_CURVE('',#3861,#3862,#2182,.T.);
#4629=EDGE_CURVE('',#3863,#3861,#2183,.T.);
#4630=EDGE_CURVE('',#3864,#3862,#2184,.T.);
#4631=EDGE_CURVE('',#3863,#3864,#2185,.T.);
#4632=EDGE_CURVE('',#3858,#3863,#2186,.T.);
#4633=EDGE_CURVE('',#3859,#3864,#2187,.T.);
#4634=EDGE_CURVE('',#3865,#3866,#2188,.T.);
#4635=EDGE_CURVE('',#3865,#3867,#2189,.T.);
#4636=EDGE_CURVE('',#3868,#3867,#2190,.T.);
#4637=EDGE_CURVE('',#3866,#3868,#2191,.T.);
#4638=EDGE_CURVE('',#3869,#3865,#2192,.T.);
#4639=EDGE_CURVE('',#3869,#3870,#2193,.T.);
#4640=EDGE_CURVE('',#3867,#3870,#2194,.T.);
#4641=EDGE_CURVE('',#3871,#3869,#2195,.T.);
#4642=EDGE_CURVE('',#3871,#3872,#2196,.T.);
#4643=EDGE_CURVE('',#3870,#3872,#2197,.T.);
#4644=EDGE_CURVE('',#3873,#3871,#2198,.T.);
#4645=EDGE_CURVE('',#3873,#3874,#2199,.T.);
#4646=EDGE_CURVE('',#3872,#3874,#2200,.T.);
#4647=EDGE_CURVE('',#3875,#3873,#2201,.T.);
#4648=EDGE_CURVE('',#3875,#3876,#2202,.T.);
#4649=EDGE_CURVE('',#3874,#3876,#2203,.T.);
#4650=EDGE_CURVE('',#3877,#3875,#2204,.T.);
#4651=EDGE_CURVE('',#3877,#3878,#2205,.T.);
#4652=EDGE_CURVE('',#3876,#3878,#2206,.T.);
#4653=EDGE_CURVE('',#3879,#3877,#2207,.T.);
#4654=EDGE_CURVE('',#3879,#3880,#2208,.T.);
#4655=EDGE_CURVE('',#3878,#3880,#2209,.T.);
#4656=EDGE_CURVE('',#3881,#3879,#2210,.T.);
#4657=EDGE_CURVE('',#3881,#3882,#2211,.T.);
#4658=EDGE_CURVE('',#3880,#3882,#2212,.T.);
#4659=EDGE_CURVE('',#3883,#3881,#2213,.T.);
#4660=EDGE_CURVE('',#3884,#3883,#2214,.T.);
#4661=EDGE_CURVE('',#3882,#3884,#2215,.T.);
#4662=EDGE_CURVE('',#3885,#3886,#2216,.T.);
#4663=EDGE_CURVE('',#3885,#3887,#2217,.T.);
#4664=EDGE_CURVE('',#3888,#3887,#2218,.T.);
#4665=EDGE_CURVE('',#3886,#3888,#2219,.T.);
#4666=EDGE_CURVE('',#3889,#3885,#2220,.T.);
#4667=EDGE_CURVE('',#3889,#3890,#2221,.T.);
#4668=EDGE_CURVE('',#3887,#3890,#2222,.T.);
#4669=EDGE_CURVE('',#3891,#3889,#2223,.T.);
#4670=EDGE_CURVE('',#3891,#3892,#2224,.T.);
#4671=EDGE_CURVE('',#3890,#3892,#2225,.T.);
#4672=EDGE_CURVE('',#3893,#3891,#2226,.T.);
#4673=EDGE_CURVE('',#3893,#3894,#2227,.T.);
#4674=EDGE_CURVE('',#3892,#3894,#2228,.T.);
#4675=EDGE_CURVE('',#3895,#3893,#2229,.T.);
#4676=EDGE_CURVE('',#3895,#3896,#2230,.T.);
#4677=EDGE_CURVE('',#3894,#3896,#2231,.T.);
#4678=EDGE_CURVE('',#3897,#3895,#2232,.T.);
#4679=EDGE_CURVE('',#3897,#3898,#2233,.T.);
#4680=EDGE_CURVE('',#3896,#3898,#2234,.T.);
#4681=EDGE_CURVE('',#3899,#3897,#2235,.T.);
#4682=EDGE_CURVE('',#3899,#3900,#2236,.T.);
#4683=EDGE_CURVE('',#3898,#3900,#2237,.T.);
#4684=EDGE_CURVE('',#3901,#3899,#2238,.T.);
#4685=EDGE_CURVE('',#3901,#3902,#2239,.T.);
#4686=EDGE_CURVE('',#3900,#3902,#2240,.T.);
#4687=EDGE_CURVE('',#3903,#3901,#2241,.T.);
#4688=EDGE_CURVE('',#3904,#3903,#2242,.T.);
#4689=EDGE_CURVE('',#3902,#3904,#2243,.T.);
#4690=EDGE_CURVE('',#3905,#3906,#2244,.T.);
#4691=EDGE_CURVE('',#3905,#3907,#2245,.T.);
#4692=EDGE_CURVE('',#3908,#3907,#2246,.T.);
#4693=EDGE_CURVE('',#3906,#3908,#2247,.T.);
#4694=EDGE_CURVE('',#3909,#3905,#2248,.T.);
#4695=EDGE_CURVE('',#3909,#3910,#2249,.T.);
#4696=EDGE_CURVE('',#3907,#3910,#2250,.T.);
#4697=EDGE_CURVE('',#3911,#3909,#2251,.T.);
#4698=EDGE_CURVE('',#3911,#3912,#2252,.T.);
#4699=EDGE_CURVE('',#3910,#3912,#2253,.T.);
#4700=EDGE_CURVE('',#3913,#3911,#2254,.T.);
#4701=EDGE_CURVE('',#3913,#3914,#2255,.T.);
#4702=EDGE_CURVE('',#3912,#3914,#2256,.T.);
#4703=EDGE_CURVE('',#3915,#3913,#2257,.T.);
#4704=EDGE_CURVE('',#3915,#3916,#2258,.T.);
#4705=EDGE_CURVE('',#3914,#3916,#2259,.T.);
#4706=EDGE_CURVE('',#3917,#3915,#2260,.T.);
#4707=EDGE_CURVE('',#3917,#3918,#2261,.T.);
#4708=EDGE_CURVE('',#3916,#3918,#2262,.T.);
#4709=EDGE_CURVE('',#3919,#3917,#2263,.T.);
#4710=EDGE_CURVE('',#3919,#3920,#2264,.T.);
#4711=EDGE_CURVE('',#3918,#3920,#2265,.T.);
#4712=EDGE_CURVE('',#3921,#3919,#2266,.T.);
#4713=EDGE_CURVE('',#3921,#3922,#2267,.T.);
#4714=EDGE_CURVE('',#3920,#3922,#2268,.T.);
#4715=EDGE_CURVE('',#3923,#3921,#2269,.T.);
#4716=EDGE_CURVE('',#3924,#3923,#2270,.T.);
#4717=EDGE_CURVE('',#3922,#3924,#2271,.T.);
#4718=EDGE_CURVE('',#3925,#3926,#2272,.T.);
#4719=EDGE_CURVE('',#3925,#3927,#2273,.T.);
#4720=EDGE_CURVE('',#3928,#3927,#2274,.T.);
#4721=EDGE_CURVE('',#3926,#3928,#2275,.T.);
#4722=EDGE_CURVE('',#3929,#3925,#2276,.T.);
#4723=EDGE_CURVE('',#3929,#3930,#2277,.T.);
#4724=EDGE_CURVE('',#3927,#3930,#2278,.T.);
#4725=EDGE_CURVE('',#3931,#3929,#2279,.T.);
#4726=EDGE_CURVE('',#3931,#3932,#2280,.T.);
#4727=EDGE_CURVE('',#3930,#3932,#2281,.T.);
#4728=EDGE_CURVE('',#3933,#3931,#2282,.T.);
#4729=EDGE_CURVE('',#3933,#3934,#2283,.T.);
#4730=EDGE_CURVE('',#3932,#3934,#2284,.T.);
#4731=EDGE_CURVE('',#3935,#3933,#2285,.T.);
#4732=EDGE_CURVE('',#3935,#3936,#2286,.T.);
#4733=EDGE_CURVE('',#3934,#3936,#2287,.T.);
#4734=EDGE_CURVE('',#3937,#3935,#2288,.T.);
#4735=EDGE_CURVE('',#3937,#3938,#2289,.T.);
#4736=EDGE_CURVE('',#3936,#3938,#2290,.T.);
#4737=EDGE_CURVE('',#3939,#3937,#2291,.T.);
#4738=EDGE_CURVE('',#3939,#3940,#2292,.T.);
#4739=EDGE_CURVE('',#3938,#3940,#2293,.T.);
#4740=EDGE_CURVE('',#3941,#3939,#2294,.T.);
#4741=EDGE_CURVE('',#3941,#3942,#2295,.T.);
#4742=EDGE_CURVE('',#3940,#3942,#2296,.T.);
#4743=EDGE_CURVE('',#3943,#3941,#2297,.T.);
#4744=EDGE_CURVE('',#3944,#3943,#2298,.T.);
#4745=EDGE_CURVE('',#3942,#3944,#2299,.T.);
#4746=EDGE_CURVE('',#3945,#3945,#3494,.T.);
#4747=EDGE_CURVE('',#3945,#3946,#2300,.T.);
#4748=EDGE_CURVE('',#3946,#3946,#3495,.T.);
#4749=EDGE_CURVE('',#3883,#3947,#2301,.T.);
#4750=EDGE_CURVE('',#3947,#3948,#2302,.T.);
#4751=EDGE_CURVE('',#3884,#3948,#2303,.T.);
#4752=EDGE_CURVE('',#3949,#3868,#2304,.T.);
#4753=EDGE_CURVE('',#3950,#3949,#2305,.T.);
#4754=EDGE_CURVE('',#3950,#3866,#2306,.T.);
#4755=EDGE_CURVE('',#3903,#3950,#2307,.T.);
#4756=EDGE_CURVE('',#3904,#3949,#2308,.T.);
#4757=EDGE_CURVE('',#3951,#3888,#2309,.T.);
#4758=EDGE_CURVE('',#3952,#3951,#2310,.T.);
#4759=EDGE_CURVE('',#3952,#3886,#2311,.T.);
#4760=EDGE_CURVE('',#3923,#3952,#2312,.T.);
#4761=EDGE_CURVE('',#3924,#3951,#2313,.T.);
#4762=EDGE_CURVE('',#3953,#3908,#2314,.T.);
#4763=EDGE_CURVE('',#3954,#3953,#2315,.T.);
#4764=EDGE_CURVE('',#3954,#3906,#2316,.T.);
#4765=EDGE_CURVE('',#3943,#3954,#2317,.T.);
#4766=EDGE_CURVE('',#3944,#3953,#2318,.T.);
#4767=EDGE_CURVE('',#3948,#3928,#2319,.T.);
#4768=EDGE_CURVE('',#3947,#3926,#2320,.T.);
#4769=EDGE_CURVE('',#3955,#3955,#3496,.T.);
#4770=EDGE_CURVE('',#3956,#3956,#3497,.T.);
#4771=EDGE_CURVE('',#3956,#3955,#2321,.T.);
#4772=EDGE_CURVE('',#3957,#3957,#3498,.T.);
#4773=EDGE_CURVE('',#3957,#3956,#2322,.T.);
#4774=EDGE_CURVE('',#3958,#3958,#3499,.T.);
#4775=EDGE_CURVE('',#3958,#3957,#2323,.T.);
#4776=EDGE_CURVE('',#3959,#3959,#3500,.T.);
#4777=EDGE_CURVE('',#3960,#3960,#3501,.F.);
#4778=EDGE_CURVE('',#3960,#3959,#2324,.T.);
#4779=EDGE_CURVE('',#3961,#3961,#3502,.F.);
#4780=EDGE_CURVE('',#3961,#3960,#2325,.T.);
#4781=EDGE_CURVE('',#3962,#3962,#3503,.T.);
#4782=EDGE_CURVE('',#3962,#3961,#2326,.T.);
#4783=EDGE_CURVE('',#3963,#3964,#2327,.T.);
#4784=EDGE_CURVE('',#3964,#3965,#2328,.T.);
#4785=EDGE_CURVE('',#3965,#3966,#2329,.T.);
#4786=EDGE_CURVE('',#3963,#3966,#2330,.T.);
#4787=EDGE_CURVE('',#3964,#3967,#2331,.T.);
#4788=EDGE_CURVE('',#3967,#3968,#2332,.T.);
#4789=EDGE_CURVE('',#3968,#3965,#2333,.T.);
#4790=EDGE_CURVE('',#3967,#3969,#2334,.T.);
#4791=EDGE_CURVE('',#3969,#3970,#2335,.T.);
#4792=EDGE_CURVE('',#3970,#3968,#2336,.T.);
#4793=EDGE_CURVE('',#3969,#3971,#2337,.T.);
#4794=EDGE_CURVE('',#3971,#3972,#2338,.T.);
#4795=EDGE_CURVE('',#3972,#3970,#2339,.T.);
#4796=EDGE_CURVE('',#3971,#3973,#2340,.T.);
#4797=EDGE_CURVE('',#3973,#3974,#2341,.T.);
#4798=EDGE_CURVE('',#3974,#3972,#2342,.T.);
#4799=EDGE_CURVE('',#3973,#3963,#2343,.T.);
#4800=EDGE_CURVE('',#3966,#3974,#2344,.T.);
#4801=EDGE_CURVE('',#3975,#3975,#3504,.T.);
#4802=EDGE_CURVE('',#3975,#3976,#2345,.T.);
#4803=EDGE_CURVE('',#3976,#3976,#3505,.T.);
#4804=EDGE_CURVE('',#3977,#3977,#3506,.T.);
#4805=EDGE_CURVE('',#3978,#3978,#3507,.T.);
#4806=EDGE_CURVE('',#3978,#3979,#2346,.T.);
#4807=EDGE_CURVE('',#3979,#3979,#3508,.T.);
#4808=EDGE_CURVE('',#3980,#3980,#3509,.T.);
#4809=EDGE_CURVE('',#3981,#3981,#3510,.T.);
#4810=EDGE_CURVE('',#3981,#3982,#2347,.T.);
#4811=EDGE_CURVE('',#3982,#3982,#3511,.T.);
#4812=EDGE_CURVE('',#3983,#3983,#3512,.T.);
#4813=EDGE_CURVE('',#3984,#3984,#3513,.T.);
#4814=EDGE_CURVE('',#3984,#3985,#2348,.T.);
#4815=EDGE_CURVE('',#3985,#3985,#3514,.T.);
#4816=EDGE_CURVE('',#3986,#3986,#3515,.T.);
#4817=EDGE_CURVE('',#3987,#3987,#3516,.T.);
#4818=EDGE_CURVE('',#3987,#3977,#2349,.T.);
#4819=EDGE_CURVE('',#3988,#3988,#3517,.T.);
#4820=EDGE_CURVE('',#3988,#3980,#2350,.T.);
#4821=EDGE_CURVE('',#3989,#3989,#3518,.T.);
#4822=EDGE_CURVE('',#3989,#3983,#2351,.T.);
#4823=EDGE_CURVE('',#3990,#3990,#3519,.T.);
#4824=EDGE_CURVE('',#3990,#3986,#2352,.T.);
#4825=EDGE_CURVE('',#3991,#3992,#2353,.T.);
#4826=EDGE_CURVE('',#3992,#3993,#2354,.T.);
#4827=EDGE_CURVE('',#3994,#3993,#2355,.T.);
#4828=EDGE_CURVE('',#3991,#3994,#2356,.T.);
#4829=EDGE_CURVE('',#3995,#3991,#2357,.T.);
#4830=EDGE_CURVE('',#3996,#3994,#2358,.T.);
#4831=EDGE_CURVE('',#3995,#3996,#2359,.T.);
#4832=EDGE_CURVE('',#3997,#3995,#2360,.T.);
#4833=EDGE_CURVE('',#3998,#3996,#2361,.T.);
#4834=EDGE_CURVE('',#3997,#3998,#2362,.T.);
#4835=EDGE_CURVE('',#3999,#3997,#2363,.T.);
#4836=EDGE_CURVE('',#4000,#3998,#2364,.T.);
#4837=EDGE_CURVE('',#3999,#4000,#2365,.T.);
#4838=EDGE_CURVE('',#4001,#3999,#2366,.T.);
#4839=EDGE_CURVE('',#4002,#4000,#2367,.T.);
#4840=EDGE_CURVE('',#4001,#4002,#2368,.T.);
#4841=EDGE_CURVE('',#4003,#4001,#2369,.T.);
#4842=EDGE_CURVE('',#4004,#4002,#2370,.T.);
#4843=EDGE_CURVE('',#4003,#4004,#2371,.T.);
#4844=EDGE_CURVE('',#4005,#4003,#2372,.T.);
#4845=EDGE_CURVE('',#4006,#4004,#2373,.T.);
#4846=EDGE_CURVE('',#4005,#4006,#2374,.T.);
#4847=EDGE_CURVE('',#4007,#4005,#2375,.T.);
#4848=EDGE_CURVE('',#4008,#4006,#2376,.T.);
#4849=EDGE_CURVE('',#4007,#4008,#2377,.T.);
#4850=EDGE_CURVE('',#4009,#4007,#2378,.T.);
#4851=EDGE_CURVE('',#4010,#4008,#2379,.T.);
#4852=EDGE_CURVE('',#4009,#4010,#2380,.T.);
#4853=EDGE_CURVE('',#4011,#4009,#2381,.T.);
#4854=EDGE_CURVE('',#4012,#4010,#2382,.T.);
#4855=EDGE_CURVE('',#4011,#4012,#2383,.T.);
#4856=EDGE_CURVE('',#4013,#4011,#2384,.T.);
#4857=EDGE_CURVE('',#4014,#4012,#2385,.T.);
#4858=EDGE_CURVE('',#4013,#4014,#2386,.T.);
#4859=EDGE_CURVE('',#3992,#4013,#2387,.T.);
#4860=EDGE_CURVE('',#3993,#4014,#2388,.T.);
#4861=EDGE_CURVE('',#4015,#4016,#2389,.T.);
#4862=EDGE_CURVE('',#4017,#4015,#2390,.T.);
#4863=EDGE_CURVE('',#4018,#4017,#2391,.T.);
#4864=EDGE_CURVE('',#4016,#4018,#2392,.T.);
#4865=EDGE_CURVE('',#4017,#4019,#2393,.T.);
#4866=EDGE_CURVE('',#4020,#4019,#2394,.T.);
#4867=EDGE_CURVE('',#4018,#4020,#2395,.T.);
#4868=EDGE_CURVE('',#4019,#4021,#2396,.T.);
#4869=EDGE_CURVE('',#4021,#4022,#2397,.T.);
#4870=EDGE_CURVE('',#4022,#4020,#2398,.T.);
#4871=EDGE_CURVE('',#4023,#4023,#3520,.T.);
#4872=EDGE_CURVE('',#4024,#4015,#2399,.T.);
#4873=EDGE_CURVE('',#4025,#4024,#2400,.T.);
#4874=EDGE_CURVE('',#4025,#4026,#2401,.T.);
#4875=EDGE_CURVE('',#4027,#4026,#2402,.T.);
#4876=EDGE_CURVE('',#4027,#4028,#2403,.T.);
#4877=EDGE_CURVE('',#4028,#4029,#2404,.T.);
#4878=EDGE_CURVE('',#4029,#4021,#2405,.T.);
#4879=EDGE_CURVE('',#4029,#4030,#2406,.T.);
#4880=EDGE_CURVE('',#4030,#4022,#2407,.T.);
#4881=EDGE_CURVE('',#4031,#4028,#2408,.T.);
#4882=EDGE_CURVE('',#4030,#4031,#2409,.T.);
#4883=EDGE_CURVE('',#4032,#4031,#2410,.T.);
#4884=EDGE_CURVE('',#4033,#4032,#2411,.T.);
#4885=EDGE_CURVE('',#4033,#4034,#2412,.T.);
#4886=EDGE_CURVE('',#4035,#4034,#2413,.T.);
#4887=EDGE_CURVE('',#4035,#4016,#2414,.T.);
#4888=EDGE_CURVE('',#4032,#4027,#2415,.T.);
#4889=EDGE_CURVE('',#4026,#4036,#2416,.T.);
#4890=EDGE_CURVE('',#4036,#4037,#323,.T.);
#4891=EDGE_CURVE('',#4037,#4033,#2417,.T.);
#4892=EDGE_CURVE('',#4038,#4036,#3521,.F.);
#4893=EDGE_CURVE('',#4038,#4023,#2418,.T.);
#4894=EDGE_CURVE('',#4039,#4038,#3522,.F.);
#4895=EDGE_CURVE('',#4040,#4039,#324,.T.);
#4896=EDGE_CURVE('',#4037,#4040,#3523,.F.);
#4897=EDGE_CURVE('',#4039,#4025,#2419,.T.);
#4898=EDGE_CURVE('',#4034,#4040,#2420,.T.);
#4899=EDGE_CURVE('',#4024,#4035,#2421,.T.);
#4900=EDGE_CURVE('',#4041,#4041,#3524,.T.);
#4901=EDGE_CURVE('',#4041,#4042,#2422,.T.);
#4902=EDGE_CURVE('',#4042,#4042,#3525,.T.);
#4903=EDGE_CURVE('',#4042,#4043,#2423,.T.);
#4904=EDGE_CURVE('',#4043,#4043,#3526,.T.);
#4905=EDGE_CURVE('',#4044,#4044,#3527,.T.);
#4906=EDGE_CURVE('',#4044,#4045,#2424,.T.);
#4907=EDGE_CURVE('',#4045,#4045,#3528,.T.);
#4908=EDGE_CURVE('',#4046,#4047,#2425,.T.);
#4909=EDGE_CURVE('',#4047,#4048,#2426,.T.);
#4910=EDGE_CURVE('',#4048,#4049,#2427,.T.);
#4911=EDGE_CURVE('',#4046,#4049,#2428,.T.);
#4912=EDGE_CURVE('',#4047,#4050,#2429,.T.);
#4913=EDGE_CURVE('',#4050,#4051,#2430,.T.);
#4914=EDGE_CURVE('',#4051,#4048,#2431,.T.);
#4915=EDGE_CURVE('',#4050,#4052,#2432,.T.);
#4916=EDGE_CURVE('',#4052,#4053,#2433,.T.);
#4917=EDGE_CURVE('',#4053,#4051,#2434,.T.);
#4918=EDGE_CURVE('',#4052,#4054,#2435,.T.);
#4919=EDGE_CURVE('',#4054,#4055,#2436,.T.);
#4920=EDGE_CURVE('',#4055,#4053,#2437,.T.);
#4921=EDGE_CURVE('',#4054,#4056,#2438,.T.);
#4922=EDGE_CURVE('',#4056,#4057,#2439,.T.);
#4923=EDGE_CURVE('',#4057,#4055,#2440,.T.);
#4924=EDGE_CURVE('',#4056,#4046,#2441,.T.);
#4925=EDGE_CURVE('',#4049,#4057,#2442,.T.);
#4926=EDGE_CURVE('',#4058,#4058,#3529,.T.);
#4927=EDGE_CURVE('',#4059,#4059,#3530,.T.);
#4928=EDGE_CURVE('',#4058,#4060,#2443,.T.);
#4929=EDGE_CURVE('',#4060,#4060,#3531,.T.);
#4930=EDGE_CURVE('',#4061,#4061,#3532,.T.);
#4931=EDGE_CURVE('',#4062,#4062,#3533,.T.);
#4932=EDGE_CURVE('',#4062,#4061,#2444,.T.);
#4933=EDGE_CURVE('',#4063,#4063,#3534,.T.);
#4934=EDGE_CURVE('',#4063,#4062,#2445,.T.);
#4935=EDGE_CURVE('',#4064,#4064,#3535,.T.);
#4936=EDGE_CURVE('',#4064,#4063,#2446,.T.);
#4937=EDGE_CURVE('',#4065,#4065,#3536,.T.);
#4938=EDGE_CURVE('',#4066,#4066,#3537,.F.);
#4939=EDGE_CURVE('',#4066,#4065,#2447,.T.);
#4940=EDGE_CURVE('',#4059,#4066,#2448,.T.);
#4941=EDGE_CURVE('',#4067,#4067,#3538,.T.);
#4942=EDGE_CURVE('',#4067,#4068,#2449,.T.);
#4943=EDGE_CURVE('',#4068,#4068,#3539,.T.);
#4944=EDGE_CURVE('',#4069,#4069,#3540,.T.);
#4945=EDGE_CURVE('',#4069,#4070,#2450,.T.);
#4946=EDGE_CURVE('',#4070,#4070,#3541,.T.);
#4947=EDGE_CURVE('',#4071,#4071,#3542,.T.);
#4948=EDGE_CURVE('',#4071,#4072,#2451,.T.);
#4949=EDGE_CURVE('',#4072,#4072,#3543,.T.);
#4950=EDGE_CURVE('',#4073,#4073,#3544,.T.);
#4951=EDGE_CURVE('',#4073,#4074,#2452,.T.);
#4952=EDGE_CURVE('',#4074,#4074,#3545,.T.);
#4953=EDGE_CURVE('',#4075,#4075,#3546,.T.);
#4954=EDGE_CURVE('',#4075,#4076,#2453,.T.);
#4955=EDGE_CURVE('',#4076,#4076,#3547,.T.);
#4956=EDGE_CURVE('',#4077,#4077,#3548,.T.);
#4957=EDGE_CURVE('',#4077,#4078,#2454,.T.);
#4958=EDGE_CURVE('',#4078,#4078,#3549,.T.);
#4959=EDGE_CURVE('',#4079,#4080,#2455,.T.);
#4960=EDGE_CURVE('',#4081,#4079,#2456,.T.);
#4961=EDGE_CURVE('',#4082,#4081,#2457,.T.);
#4962=EDGE_CURVE('',#4082,#4080,#2458,.T.);
#4963=EDGE_CURVE('',#4083,#4084,#2459,.T.);
#4964=EDGE_CURVE('',#4083,#4085,#2460,.T.);
#4965=EDGE_CURVE('',#4085,#4086,#2461,.T.);
#4966=EDGE_CURVE('',#4084,#4086,#2462,.T.);
#4967=EDGE_CURVE('',#4085,#4082,#2463,.T.);
#4968=EDGE_CURVE('',#4086,#4081,#2464,.T.);
#4969=EDGE_CURVE('',#4087,#4083,#2465,.T.);
#4970=EDGE_CURVE('',#4088,#4087,#2466,.T.);
#4971=EDGE_CURVE('',#4089,#4088,#2467,.T.);
#4972=EDGE_CURVE('',#4090,#4089,#2468,.T.);
#4973=EDGE_CURVE('',#4080,#4090,#2469,.T.);
#4974=EDGE_CURVE('',#4091,#4084,#2470,.T.);
#4975=EDGE_CURVE('',#4087,#4091,#2471,.T.);
#4976=EDGE_CURVE('',#4089,#4092,#2472,.T.);
#4977=EDGE_CURVE('',#4093,#4092,#2473,.T.);
#4978=EDGE_CURVE('',#4090,#4093,#2474,.T.);
#4979=EDGE_CURVE('',#4079,#4093,#2475,.T.);
#4980=EDGE_CURVE('',#4094,#4091,#2476,.T.);
#4981=EDGE_CURVE('',#4088,#4094,#2477,.T.);
#4982=EDGE_CURVE('',#4092,#4094,#2478,.T.);
#4983=EDGE_CURVE('',#4095,#4095,#3550,.T.);
#4984=EDGE_CURVE('',#4095,#4096,#2479,.T.);
#4985=EDGE_CURVE('',#4096,#4096,#3551,.T.);
#4986=EDGE_CURVE('',#4097,#4097,#3552,.T.);
#4987=EDGE_CURVE('',#4097,#4098,#2480,.T.);
#4988=EDGE_CURVE('',#4098,#4098,#3553,.T.);
#4989=EDGE_CURVE('',#4099,#4099,#3554,.T.);
#4990=EDGE_CURVE('',#4099,#4100,#2481,.T.);
#4991=EDGE_CURVE('',#4101,#4100,#325,.T.);
#4992=EDGE_CURVE('',#4101,#4100,#3555,.T.);
#4993=EDGE_CURVE('',#4100,#4101,#2482,.T.);
#4994=EDGE_CURVE('',#4101,#4102,#3556,.T.);
#4995=EDGE_CURVE('',#4102,#4100,#3557,.T.);
#4996=EDGE_CURVE('',#4103,#4103,#3558,.T.);
#4997=EDGE_CURVE('',#4103,#4104,#2483,.T.);
#4998=EDGE_CURVE('',#4104,#4105,#3559,.T.);
#4999=EDGE_CURVE('',#4104,#4105,#326,.T.);
#5000=EDGE_CURVE('',#4105,#4104,#2484,.T.);
#5001=EDGE_CURVE('',#4106,#4104,#3560,.T.);
#5002=EDGE_CURVE('',#4105,#4106,#3561,.T.);
#5003=EDGE_CURVE('',#4102,#4106,#2485,.T.);
#5004=EDGE_CURVE('',#4107,#4108,#2486,.T.);
#5005=EDGE_CURVE('',#4107,#4108,#3562,.T.);
#5006=EDGE_CURVE('',#4109,#4107,#2487,.T.);
#5007=EDGE_CURVE('',#4110,#4109,#3563,.T.);
#5008=EDGE_CURVE('',#4110,#4111,#2488,.T.);
#5009=EDGE_CURVE('',#4111,#4111,#3564,.T.);
#5010=EDGE_CURVE('',#4112,#4110,#3565,.T.);
#5011=EDGE_CURVE('',#4108,#4112,#2489,.T.);
#5012=EDGE_CURVE('',#4113,#4114,#2490,.T.);
#5013=EDGE_CURVE('',#4113,#4114,#3566,.T.);
#5014=EDGE_CURVE('',#4115,#4113,#2491,.T.);
#5015=EDGE_CURVE('',#4116,#4115,#3567,.T.);
#5016=EDGE_CURVE('',#4116,#4117,#2492,.T.);
#5017=EDGE_CURVE('',#4117,#4117,#3568,.T.);
#5018=EDGE_CURVE('',#4118,#4116,#3569,.T.);
#5019=EDGE_CURVE('',#4114,#4118,#2493,.T.);
#5020=EDGE_CURVE('',#4119,#4120,#2494,.T.);
#5021=EDGE_CURVE('',#4119,#4120,#3570,.T.);
#5022=EDGE_CURVE('',#4121,#4119,#2495,.T.);
#5023=EDGE_CURVE('',#4122,#4121,#3571,.T.);
#5024=EDGE_CURVE('',#4122,#4123,#2496,.T.);
#5025=EDGE_CURVE('',#4123,#4123,#3572,.T.);
#5026=EDGE_CURVE('',#4124,#4122,#3573,.T.);
#5027=EDGE_CURVE('',#4120,#4124,#2497,.T.);
#5028=EDGE_CURVE('',#4125,#4126,#2498,.T.);
#5029=EDGE_CURVE('',#4125,#4126,#3574,.T.);
#5030=EDGE_CURVE('',#4127,#4125,#2499,.T.);
#5031=EDGE_CURVE('',#4128,#4127,#3575,.T.);
#5032=EDGE_CURVE('',#4128,#4129,#2500,.T.);
#5033=EDGE_CURVE('',#4129,#4129,#3576,.T.);
#5034=EDGE_CURVE('',#4130,#4128,#3577,.T.);
#5035=EDGE_CURVE('',#4126,#4130,#2501,.T.);
#5036=EDGE_CURVE('',#4112,#4121,#2502,.T.);
#5037=EDGE_CURVE('',#4124,#4131,#2503,.T.);
#5038=EDGE_CURVE('',#4132,#4131,#2504,.T.);
#5039=EDGE_CURVE('',#4132,#4133,#2505,.T.);
#5040=EDGE_CURVE('',#4134,#4133,#2506,.T.);
#5041=EDGE_CURVE('',#4134,#4109,#2507,.T.);
#5042=EDGE_CURVE('',#4118,#4127,#2508,.T.);
#5043=EDGE_CURVE('',#4130,#4135,#2509,.T.);
#5044=EDGE_CURVE('',#4136,#4135,#2510,.T.);
#5045=EDGE_CURVE('',#4137,#4136,#2511,.T.);
#5046=EDGE_CURVE('',#4138,#4137,#2512,.T.);
#5047=EDGE_CURVE('',#4138,#4115,#2513,.T.);
#5048=EDGE_CURVE('',#4131,#4139,#2514,.T.);
#5049=EDGE_CURVE('',#4139,#4140,#2515,.T.);
#5050=EDGE_CURVE('',#4140,#4141,#2516,.T.);
#5051=EDGE_CURVE('',#4141,#4142,#2517,.T.);
#5052=EDGE_CURVE('',#4142,#4138,#2518,.T.);
#5053=EDGE_CURVE('',#4137,#4143,#2519,.T.);
#5054=EDGE_CURVE('',#4143,#4144,#2520,.T.);
#5055=EDGE_CURVE('',#4144,#4145,#2521,.T.);
#5056=EDGE_CURVE('',#4145,#4146,#2522,.T.);
#5057=EDGE_CURVE('',#4146,#4132,#2523,.T.);
#5058=EDGE_CURVE('',#4147,#4134,#2524,.T.);
#5059=EDGE_CURVE('',#4139,#4147,#2525,.T.);
#5060=EDGE_CURVE('',#4148,#4147,#2526,.T.);
#5061=EDGE_CURVE('',#4140,#4148,#2527,.T.);
#5062=EDGE_CURVE('',#4149,#4148,#2528,.T.);
#5063=EDGE_CURVE('',#4141,#4149,#2529,.T.);
#5064=EDGE_CURVE('',#4150,#4149,#2530,.T.);
#5065=EDGE_CURVE('',#4142,#4150,#2531,.T.);
#5066=EDGE_CURVE('',#4135,#4150,#2532,.T.);
#5067=EDGE_CURVE('',#4151,#4136,#2533,.T.);
#5068=EDGE_CURVE('',#4143,#4151,#2534,.T.);
#5069=EDGE_CURVE('',#4152,#4151,#2535,.T.);
#5070=EDGE_CURVE('',#4144,#4152,#2536,.T.);
#5071=EDGE_CURVE('',#4153,#4152,#2537,.T.);
#5072=EDGE_CURVE('',#4145,#4153,#2538,.T.);
#5073=EDGE_CURVE('',#4154,#4153,#2539,.T.);
#5074=EDGE_CURVE('',#4146,#4154,#2540,.T.);
#5075=EDGE_CURVE('',#4133,#4154,#2541,.T.);
#5076=EDGE_CURVE('',#4155,#4156,#2542,.T.);
#5077=EDGE_CURVE('',#4156,#4157,#2543,.T.);
#5078=EDGE_CURVE('',#4158,#4157,#2544,.T.);
#5079=EDGE_CURVE('',#4155,#4158,#2545,.T.);
#5080=EDGE_CURVE('',#4159,#4155,#2546,.T.);
#5081=EDGE_CURVE('',#4160,#4158,#2547,.T.);
#5082=EDGE_CURVE('',#4159,#4160,#2548,.T.);
#5083=EDGE_CURVE('',#4161,#4159,#2549,.T.);
#5084=EDGE_CURVE('',#4162,#4160,#2550,.T.);
#5085=EDGE_CURVE('',#4161,#4162,#2551,.T.);
#5086=EDGE_CURVE('',#4163,#4161,#2552,.T.);
#5087=EDGE_CURVE('',#4164,#4162,#2553,.T.);
#5088=EDGE_CURVE('',#4163,#4164,#2554,.T.);
#5089=EDGE_CURVE('',#4165,#4163,#2555,.T.);
#5090=EDGE_CURVE('',#4166,#4164,#2556,.T.);
#5091=EDGE_CURVE('',#4165,#4166,#2557,.T.);
#5092=EDGE_CURVE('',#4167,#4165,#2558,.T.);
#5093=EDGE_CURVE('',#4168,#4166,#2559,.T.);
#5094=EDGE_CURVE('',#4167,#4168,#2560,.T.);
#5095=EDGE_CURVE('',#4169,#4167,#2561,.T.);
#5096=EDGE_CURVE('',#4170,#4168,#2562,.T.);
#5097=EDGE_CURVE('',#4169,#4170,#2563,.T.);
#5098=EDGE_CURVE('',#4156,#4169,#2564,.T.);
#5099=EDGE_CURVE('',#4157,#4170,#2565,.T.);
#5100=EDGE_CURVE('',#4171,#4172,#2566,.T.);
#5101=EDGE_CURVE('',#4171,#4173,#2567,.T.);
#5102=EDGE_CURVE('',#4174,#4173,#2568,.T.);
#5103=EDGE_CURVE('',#4172,#4174,#2569,.T.);
#5104=EDGE_CURVE('',#4172,#4175,#2570,.T.);
#5105=EDGE_CURVE('',#4176,#4174,#2571,.T.);
#5106=EDGE_CURVE('',#4175,#4176,#2572,.T.);
#5107=EDGE_CURVE('',#4175,#4177,#2573,.T.);
#5108=EDGE_CURVE('',#4178,#4176,#2574,.T.);
#5109=EDGE_CURVE('',#4177,#4178,#2575,.T.);
#5110=EDGE_CURVE('',#4177,#4179,#2576,.T.);
#5111=EDGE_CURVE('',#4180,#4178,#2577,.T.);
#5112=EDGE_CURVE('',#4179,#4180,#2578,.T.);
#5113=EDGE_CURVE('',#4179,#4181,#2579,.T.);
#5114=EDGE_CURVE('',#4182,#4180,#2580,.T.);
#5115=EDGE_CURVE('',#4181,#4182,#2581,.T.);
#5116=EDGE_CURVE('',#4181,#4183,#2582,.T.);
#5117=EDGE_CURVE('',#4184,#4182,#2583,.T.);
#5118=EDGE_CURVE('',#4183,#4184,#2584,.T.);
#5119=EDGE_CURVE('',#4183,#4185,#2585,.T.);
#5120=EDGE_CURVE('',#4186,#4184,#2586,.T.);
#5121=EDGE_CURVE('',#4185,#4186,#2587,.T.);
#5122=EDGE_CURVE('',#4185,#4171,#2588,.T.);
#5123=EDGE_CURVE('',#4173,#4186,#2589,.T.);
#5124=EDGE_CURVE('',#4187,#4188,#2590,.T.);
#5125=EDGE_CURVE('',#4188,#4189,#2591,.T.);
#5126=EDGE_CURVE('',#4189,#4190,#2592,.T.);
#5127=EDGE_CURVE('',#4187,#4190,#2593,.T.);
#5128=EDGE_CURVE('',#4188,#4191,#2594,.T.);
#5129=EDGE_CURVE('',#4191,#4192,#2595,.T.);
#5130=EDGE_CURVE('',#4192,#4189,#2596,.T.);
#5131=EDGE_CURVE('',#4191,#4193,#2597,.T.);
#5132=EDGE_CURVE('',#4193,#4194,#2598,.T.);
#5133=EDGE_CURVE('',#4194,#4192,#2599,.T.);
#5134=EDGE_CURVE('',#4193,#4195,#2600,.T.);
#5135=EDGE_CURVE('',#4195,#4196,#2601,.T.);
#5136=EDGE_CURVE('',#4196,#4194,#2602,.T.);
#5137=EDGE_CURVE('',#4195,#4197,#2603,.T.);
#5138=EDGE_CURVE('',#4197,#4198,#2604,.T.);
#5139=EDGE_CURVE('',#4198,#4196,#2605,.T.);
#5140=EDGE_CURVE('',#4197,#4187,#2606,.T.);
#5141=EDGE_CURVE('',#4190,#4198,#2607,.T.);
#5142=EDGE_CURVE('',#4199,#4199,#3578,.T.);
#5143=EDGE_CURVE('',#4200,#4200,#3579,.T.);
#5144=EDGE_CURVE('',#4201,#4201,#3580,.T.);
#5145=EDGE_CURVE('',#4201,#4200,#2608,.T.);
#5146=EDGE_CURVE('',#4202,#4202,#3581,.T.);
#5147=EDGE_CURVE('',#4202,#4201,#2609,.T.);
#5148=EDGE_CURVE('',#4203,#4203,#3582,.T.);
#5149=EDGE_CURVE('',#4203,#4202,#2610,.T.);
#5150=EDGE_CURVE('',#4204,#4204,#3583,.T.);
#5151=EDGE_CURVE('',#4205,#4205,#3584,.F.);
#5152=EDGE_CURVE('',#4205,#4204,#2611,.T.);
#5153=EDGE_CURVE('',#4199,#4205,#2612,.T.);
#5154=EDGE_CURVE('',#4206,#4206,#3585,.T.);
#5155=EDGE_CURVE('',#4207,#4207,#3586,.T.);
#5156=EDGE_CURVE('',#4207,#4206,#2613,.T.);
#5157=EDGE_CURVE('',#4208,#4208,#3587,.T.);
#5158=EDGE_CURVE('',#4208,#4207,#2614,.T.);
#5159=EDGE_CURVE('',#4209,#4209,#3588,.T.);
#5160=EDGE_CURVE('',#4209,#4208,#2615,.T.);
#5161=EDGE_CURVE('',#4210,#4210,#3589,.T.);
#5162=EDGE_CURVE('',#4211,#4211,#3590,.F.);
#5163=EDGE_CURVE('',#4211,#4210,#2616,.T.);
#5164=EDGE_CURVE('',#4212,#4212,#3591,.F.);
#5165=EDGE_CURVE('',#4212,#4211,#2617,.T.);
#5166=EDGE_CURVE('',#4213,#4213,#3592,.T.);
#5167=EDGE_CURVE('',#4213,#4212,#2618,.T.);
#5168=EDGE_CURVE('',#4214,#4215,#2619,.T.);
#5169=EDGE_CURVE('',#4215,#4216,#2620,.T.);
#5170=EDGE_CURVE('',#4216,#4217,#2621,.T.);
#5171=EDGE_CURVE('',#4214,#4217,#2622,.T.);
#5172=EDGE_CURVE('',#4215,#4218,#2623,.T.);
#5173=EDGE_CURVE('',#4218,#4219,#2624,.T.);
#5174=EDGE_CURVE('',#4219,#4216,#2625,.T.);
#5175=EDGE_CURVE('',#4218,#4220,#2626,.T.);
#5176=EDGE_CURVE('',#4220,#4221,#2627,.T.);
#5177=EDGE_CURVE('',#4221,#4219,#2628,.T.);
#5178=EDGE_CURVE('',#4220,#4222,#2629,.T.);
#5179=EDGE_CURVE('',#4222,#4223,#2630,.T.);
#5180=EDGE_CURVE('',#4223,#4221,#2631,.T.);
#5181=EDGE_CURVE('',#4222,#4224,#2632,.T.);
#5182=EDGE_CURVE('',#4224,#4225,#2633,.T.);
#5183=EDGE_CURVE('',#4225,#4223,#2634,.T.);
#5184=EDGE_CURVE('',#4224,#4214,#2635,.T.);
#5185=EDGE_CURVE('',#4217,#4225,#2636,.T.);
#5186=ORIENTED_EDGE('',*,*,#4226,.F.);
#5187=ORIENTED_EDGE('',*,*,#4227,.T.);
#5188=ORIENTED_EDGE('',*,*,#4228,.F.);
#5189=ORIENTED_EDGE('',*,*,#4227,.F.);
#5190=ORIENTED_EDGE('',*,*,#4229,.F.);
#5191=ORIENTED_EDGE('',*,*,#4230,.T.);
#5192=ORIENTED_EDGE('',*,*,#4231,.F.);
#5193=ORIENTED_EDGE('',*,*,#4230,.F.);
#5194=ORIENTED_EDGE('',*,*,#4232,.F.);
#5195=ORIENTED_EDGE('',*,*,#4233,.T.);
#5196=ORIENTED_EDGE('',*,*,#4234,.F.);
#5197=ORIENTED_EDGE('',*,*,#4233,.F.);
#5198=ORIENTED_EDGE('',*,*,#4235,.F.);
#5199=ORIENTED_EDGE('',*,*,#4236,.T.);
#5200=ORIENTED_EDGE('',*,*,#4237,.F.);
#5201=ORIENTED_EDGE('',*,*,#4236,.F.);
#5202=ORIENTED_EDGE('',*,*,#4238,.T.);
#5203=ORIENTED_EDGE('',*,*,#4239,.T.);
#5204=ORIENTED_EDGE('',*,*,#4240,.F.);
#5205=ORIENTED_EDGE('',*,*,#4241,.F.);
#5206=ORIENTED_EDGE('',*,*,#4242,.T.);
#5207=ORIENTED_EDGE('',*,*,#4241,.T.);
#5208=ORIENTED_EDGE('',*,*,#4243,.F.);
#5209=ORIENTED_EDGE('',*,*,#4244,.F.);
#5210=ORIENTED_EDGE('',*,*,#4245,.T.);
#5211=ORIENTED_EDGE('',*,*,#4244,.T.);
#5212=ORIENTED_EDGE('',*,*,#4246,.F.);
#5213=ORIENTED_EDGE('',*,*,#4247,.F.);
#5214=ORIENTED_EDGE('',*,*,#4248,.T.);
#5215=ORIENTED_EDGE('',*,*,#4247,.T.);
#5216=ORIENTED_EDGE('',*,*,#4249,.F.);
#5217=ORIENTED_EDGE('',*,*,#4239,.F.);
#5218=ORIENTED_EDGE('',*,*,#4249,.T.);
#5219=ORIENTED_EDGE('',*,*,#4246,.T.);
#5220=ORIENTED_EDGE('',*,*,#4243,.T.);
#5221=ORIENTED_EDGE('',*,*,#4240,.T.);
#5222=ORIENTED_EDGE('',*,*,#4228,.T.);
#5223=ORIENTED_EDGE('',*,*,#4231,.T.);
#5224=ORIENTED_EDGE('',*,*,#4234,.T.);
#5225=ORIENTED_EDGE('',*,*,#4237,.T.);
#5226=ORIENTED_EDGE('',*,*,#4248,.F.);
#5227=ORIENTED_EDGE('',*,*,#4238,.F.);
#5228=ORIENTED_EDGE('',*,*,#4242,.F.);
#5229=ORIENTED_EDGE('',*,*,#4245,.F.);
#5230=ORIENTED_EDGE('',*,*,#4226,.T.);
#5231=ORIENTED_EDGE('',*,*,#4229,.T.);
#5232=ORIENTED_EDGE('',*,*,#4232,.T.);
#5233=ORIENTED_EDGE('',*,*,#4235,.T.);
#5234=ORIENTED_EDGE('',*,*,#4250,.F.);
#5235=ORIENTED_EDGE('',*,*,#4251,.T.);
#5236=ORIENTED_EDGE('',*,*,#4252,.F.);
#5237=ORIENTED_EDGE('',*,*,#4251,.F.);
#5238=ORIENTED_EDGE('',*,*,#4253,.F.);
#5239=ORIENTED_EDGE('',*,*,#4254,.T.);
#5240=ORIENTED_EDGE('',*,*,#4255,.F.);
#5241=ORIENTED_EDGE('',*,*,#4254,.F.);
#5242=ORIENTED_EDGE('',*,*,#4256,.F.);
#5243=ORIENTED_EDGE('',*,*,#4257,.T.);
#5244=ORIENTED_EDGE('',*,*,#4258,.F.);
#5245=ORIENTED_EDGE('',*,*,#4257,.F.);
#5246=ORIENTED_EDGE('',*,*,#4259,.F.);
#5247=ORIENTED_EDGE('',*,*,#4260,.T.);
#5248=ORIENTED_EDGE('',*,*,#4261,.F.);
#5249=ORIENTED_EDGE('',*,*,#4260,.F.);
#5250=ORIENTED_EDGE('',*,*,#4262,.F.);
#5251=ORIENTED_EDGE('',*,*,#4263,.F.);
#5252=ORIENTED_EDGE('',*,*,#4264,.F.);
#5253=ORIENTED_EDGE('',*,*,#4265,.T.);
#5254=ORIENTED_EDGE('',*,*,#4266,.F.);
#5255=ORIENTED_EDGE('',*,*,#4265,.F.);
#5256=ORIENTED_EDGE('',*,*,#4267,.F.);
#5257=ORIENTED_EDGE('',*,*,#4268,.T.);
#5258=ORIENTED_EDGE('',*,*,#4269,.F.);
#5259=ORIENTED_EDGE('',*,*,#4268,.F.);
#5260=ORIENTED_EDGE('',*,*,#4270,.F.);
#5261=ORIENTED_EDGE('',*,*,#4271,.T.);
#5262=ORIENTED_EDGE('',*,*,#4272,.F.);
#5263=ORIENTED_EDGE('',*,*,#4271,.F.);
#5264=ORIENTED_EDGE('',*,*,#4273,.F.);
#5265=ORIENTED_EDGE('',*,*,#4263,.T.);
#5266=ORIENTED_EDGE('',*,*,#4274,.T.);
#5267=ORIENTED_EDGE('',*,*,#4275,.T.);
#5268=ORIENTED_EDGE('',*,*,#4276,.F.);
#5269=ORIENTED_EDGE('',*,*,#4277,.F.);
#5270=ORIENTED_EDGE('',*,*,#4278,.T.);
#5271=ORIENTED_EDGE('',*,*,#4277,.T.);
#5272=ORIENTED_EDGE('',*,*,#4279,.F.);
#5273=ORIENTED_EDGE('',*,*,#4280,.F.);
#5274=ORIENTED_EDGE('',*,*,#4281,.T.);
#5275=ORIENTED_EDGE('',*,*,#4280,.T.);
#5276=ORIENTED_EDGE('',*,*,#4282,.F.);
#5277=ORIENTED_EDGE('',*,*,#4283,.F.);
#5278=ORIENTED_EDGE('',*,*,#4284,.T.);
#5279=ORIENTED_EDGE('',*,*,#4283,.T.);
#5280=ORIENTED_EDGE('',*,*,#4285,.F.);
#5281=ORIENTED_EDGE('',*,*,#4275,.F.);
#5282=ORIENTED_EDGE('',*,*,#4285,.T.);
#5283=ORIENTED_EDGE('',*,*,#4282,.T.);
#5284=ORIENTED_EDGE('',*,*,#4279,.T.);
#5285=ORIENTED_EDGE('',*,*,#4276,.T.);
#5286=ORIENTED_EDGE('',*,*,#4269,.T.);
#5287=ORIENTED_EDGE('',*,*,#4272,.T.);
#5288=ORIENTED_EDGE('',*,*,#4262,.T.);
#5289=ORIENTED_EDGE('',*,*,#4266,.T.);
#5290=ORIENTED_EDGE('',*,*,#4261,.T.);
#5291=ORIENTED_EDGE('',*,*,#4258,.T.);
#5292=ORIENTED_EDGE('',*,*,#4255,.T.);
#5293=ORIENTED_EDGE('',*,*,#4252,.T.);
#5294=ORIENTED_EDGE('',*,*,#4284,.F.);
#5295=ORIENTED_EDGE('',*,*,#4274,.F.);
#5296=ORIENTED_EDGE('',*,*,#4278,.F.);
#5297=ORIENTED_EDGE('',*,*,#4281,.F.);
#5298=ORIENTED_EDGE('',*,*,#4270,.T.);
#5299=ORIENTED_EDGE('',*,*,#4267,.T.);
#5300=ORIENTED_EDGE('',*,*,#4264,.T.);
#5301=ORIENTED_EDGE('',*,*,#4273,.T.);
#5302=ORIENTED_EDGE('',*,*,#4259,.T.);
#5303=ORIENTED_EDGE('',*,*,#4256,.T.);
#5304=ORIENTED_EDGE('',*,*,#4253,.T.);
#5305=ORIENTED_EDGE('',*,*,#4250,.T.);
#5306=ORIENTED_EDGE('',*,*,#4286,.T.);
#5307=ORIENTED_EDGE('',*,*,#4287,.T.);
#5308=ORIENTED_EDGE('',*,*,#4288,.F.);
#5309=ORIENTED_EDGE('',*,*,#4289,.F.);
#5310=ORIENTED_EDGE('',*,*,#4290,.T.);
#5311=ORIENTED_EDGE('',*,*,#4289,.T.);
#5312=ORIENTED_EDGE('',*,*,#4291,.F.);
#5313=ORIENTED_EDGE('',*,*,#4292,.F.);
#5314=ORIENTED_EDGE('',*,*,#4293,.T.);
#5315=ORIENTED_EDGE('',*,*,#4292,.T.);
#5316=ORIENTED_EDGE('',*,*,#4294,.F.);
#5317=ORIENTED_EDGE('',*,*,#4295,.F.);
#5318=ORIENTED_EDGE('',*,*,#4296,.T.);
#5319=ORIENTED_EDGE('',*,*,#4295,.T.);
#5320=ORIENTED_EDGE('',*,*,#4297,.F.);
#5321=ORIENTED_EDGE('',*,*,#4287,.F.);
#5322=ORIENTED_EDGE('',*,*,#4297,.T.);
#5323=ORIENTED_EDGE('',*,*,#4294,.T.);
#5324=ORIENTED_EDGE('',*,*,#4291,.T.);
#5325=ORIENTED_EDGE('',*,*,#4288,.T.);
#5326=ORIENTED_EDGE('',*,*,#4296,.F.);
#5327=ORIENTED_EDGE('',*,*,#4286,.F.);
#5328=ORIENTED_EDGE('',*,*,#4290,.F.);
#5329=ORIENTED_EDGE('',*,*,#4293,.F.);
#5330=ORIENTED_EDGE('',*,*,#4298,.T.);
#5331=ORIENTED_EDGE('',*,*,#4299,.T.);
#5332=ORIENTED_EDGE('',*,*,#4300,.F.);
#5333=ORIENTED_EDGE('',*,*,#4301,.F.);
#5334=ORIENTED_EDGE('',*,*,#4302,.T.);
#5335=ORIENTED_EDGE('',*,*,#4301,.T.);
#5336=ORIENTED_EDGE('',*,*,#4303,.F.);
#5337=ORIENTED_EDGE('',*,*,#4304,.F.);
#5338=ORIENTED_EDGE('',*,*,#4305,.T.);
#5339=ORIENTED_EDGE('',*,*,#4304,.T.);
#5340=ORIENTED_EDGE('',*,*,#4306,.F.);
#5341=ORIENTED_EDGE('',*,*,#4307,.F.);
#5342=ORIENTED_EDGE('',*,*,#4308,.T.);
#5343=ORIENTED_EDGE('',*,*,#4307,.T.);
#5344=ORIENTED_EDGE('',*,*,#4309,.F.);
#5345=ORIENTED_EDGE('',*,*,#4299,.F.);
#5346=ORIENTED_EDGE('',*,*,#4309,.T.);
#5347=ORIENTED_EDGE('',*,*,#4306,.T.);
#5348=ORIENTED_EDGE('',*,*,#4303,.T.);
#5349=ORIENTED_EDGE('',*,*,#4300,.T.);
#5350=ORIENTED_EDGE('',*,*,#4308,.F.);
#5351=ORIENTED_EDGE('',*,*,#4298,.F.);
#5352=ORIENTED_EDGE('',*,*,#4302,.F.);
#5353=ORIENTED_EDGE('',*,*,#4305,.F.);
#5354=ORIENTED_EDGE('',*,*,#4310,.F.);
#5355=ORIENTED_EDGE('',*,*,#4311,.T.);
#5356=ORIENTED_EDGE('',*,*,#4312,.F.);
#5357=ORIENTED_EDGE('',*,*,#4313,.F.);
#5358=ORIENTED_EDGE('',*,*,#4314,.F.);
#5359=ORIENTED_EDGE('',*,*,#4313,.T.);
#5360=ORIENTED_EDGE('',*,*,#4315,.F.);
#5361=ORIENTED_EDGE('',*,*,#4316,.F.);
#5362=ORIENTED_EDGE('',*,*,#4317,.F.);
#5363=ORIENTED_EDGE('',*,*,#4316,.T.);
#5364=ORIENTED_EDGE('',*,*,#4318,.F.);
#5365=ORIENTED_EDGE('',*,*,#4319,.F.);
#5366=ORIENTED_EDGE('',*,*,#4320,.F.);
#5367=ORIENTED_EDGE('',*,*,#4319,.T.);
#5368=ORIENTED_EDGE('',*,*,#4321,.F.);
#5369=ORIENTED_EDGE('',*,*,#4311,.F.);
#5370=ORIENTED_EDGE('',*,*,#4321,.T.);
#5371=ORIENTED_EDGE('',*,*,#4318,.T.);
#5372=ORIENTED_EDGE('',*,*,#4315,.T.);
#5373=ORIENTED_EDGE('',*,*,#4312,.T.);
#5374=ORIENTED_EDGE('',*,*,#4320,.T.);
#5375=ORIENTED_EDGE('',*,*,#4310,.T.);
#5376=ORIENTED_EDGE('',*,*,#4314,.T.);
#5377=ORIENTED_EDGE('',*,*,#4317,.T.);
#5378=ORIENTED_EDGE('',*,*,#4322,.F.);
#5379=ORIENTED_EDGE('',*,*,#4323,.T.);
#5380=ORIENTED_EDGE('',*,*,#4324,.F.);
#5381=ORIENTED_EDGE('',*,*,#4323,.F.);
#5382=ORIENTED_EDGE('',*,*,#4325,.F.);
#5383=ORIENTED_EDGE('',*,*,#4326,.T.);
#5384=ORIENTED_EDGE('',*,*,#4327,.F.);
#5385=ORIENTED_EDGE('',*,*,#4326,.F.);
#5386=ORIENTED_EDGE('',*,*,#4328,.F.);
#5387=ORIENTED_EDGE('',*,*,#4329,.T.);
#5388=ORIENTED_EDGE('',*,*,#4330,.F.);
#5389=ORIENTED_EDGE('',*,*,#4331,.F.);
#5390=ORIENTED_EDGE('',*,*,#4332,.F.);
#5391=ORIENTED_EDGE('',*,*,#4331,.T.);
#5392=ORIENTED_EDGE('',*,*,#4333,.F.);
#5393=ORIENTED_EDGE('',*,*,#4334,.F.);
#5394=ORIENTED_EDGE('',*,*,#4335,.F.);
#5395=ORIENTED_EDGE('',*,*,#4334,.T.);
#5396=ORIENTED_EDGE('',*,*,#4336,.F.);
#5397=ORIENTED_EDGE('',*,*,#4337,.F.);
#5398=ORIENTED_EDGE('',*,*,#4338,.F.);
#5399=ORIENTED_EDGE('',*,*,#4337,.T.);
#5400=ORIENTED_EDGE('',*,*,#4339,.F.);
#5401=ORIENTED_EDGE('',*,*,#4329,.F.);
#5402=ORIENTED_EDGE('',*,*,#4339,.T.);
#5403=ORIENTED_EDGE('',*,*,#4336,.T.);
#5404=ORIENTED_EDGE('',*,*,#4333,.T.);
#5405=ORIENTED_EDGE('',*,*,#4330,.T.);
#5406=ORIENTED_EDGE('',*,*,#4324,.T.);
#5407=ORIENTED_EDGE('',*,*,#4327,.T.);
#5408=ORIENTED_EDGE('',*,*,#4338,.T.);
#5409=ORIENTED_EDGE('',*,*,#4328,.T.);
#5410=ORIENTED_EDGE('',*,*,#4332,.T.);
#5411=ORIENTED_EDGE('',*,*,#4335,.T.);
#5412=ORIENTED_EDGE('',*,*,#4322,.T.);
#5413=ORIENTED_EDGE('',*,*,#4325,.T.);
#5414=ORIENTED_EDGE('',*,*,#4340,.F.);
#5415=ORIENTED_EDGE('',*,*,#4341,.T.);
#5416=ORIENTED_EDGE('',*,*,#4342,.F.);
#5417=ORIENTED_EDGE('',*,*,#4341,.F.);
#5418=ORIENTED_EDGE('',*,*,#4343,.F.);
#5419=ORIENTED_EDGE('',*,*,#4344,.T.);
#5420=ORIENTED_EDGE('',*,*,#4345,.F.);
#5421=ORIENTED_EDGE('',*,*,#4344,.F.);
#5422=ORIENTED_EDGE('',*,*,#4346,.F.);
#5423=ORIENTED_EDGE('',*,*,#4347,.T.);
#5424=ORIENTED_EDGE('',*,*,#4348,.F.);
#5425=ORIENTED_EDGE('',*,*,#4349,.F.);
#5426=ORIENTED_EDGE('',*,*,#4350,.F.);
#5427=ORIENTED_EDGE('',*,*,#4349,.T.);
#5428=ORIENTED_EDGE('',*,*,#4351,.F.);
#5429=ORIENTED_EDGE('',*,*,#4352,.F.);
#5430=ORIENTED_EDGE('',*,*,#4353,.F.);
#5431=ORIENTED_EDGE('',*,*,#4352,.T.);
#5432=ORIENTED_EDGE('',*,*,#4354,.F.);
#5433=ORIENTED_EDGE('',*,*,#4355,.F.);
#5434=ORIENTED_EDGE('',*,*,#4356,.F.);
#5435=ORIENTED_EDGE('',*,*,#4355,.T.);
#5436=ORIENTED_EDGE('',*,*,#4357,.F.);
#5437=ORIENTED_EDGE('',*,*,#4347,.F.);
#5438=ORIENTED_EDGE('',*,*,#4357,.T.);
#5439=ORIENTED_EDGE('',*,*,#4354,.T.);
#5440=ORIENTED_EDGE('',*,*,#4351,.T.);
#5441=ORIENTED_EDGE('',*,*,#4348,.T.);
#5442=ORIENTED_EDGE('',*,*,#4342,.T.);
#5443=ORIENTED_EDGE('',*,*,#4345,.T.);
#5444=ORIENTED_EDGE('',*,*,#4356,.T.);
#5445=ORIENTED_EDGE('',*,*,#4346,.T.);
#5446=ORIENTED_EDGE('',*,*,#4350,.T.);
#5447=ORIENTED_EDGE('',*,*,#4353,.T.);
#5448=ORIENTED_EDGE('',*,*,#4340,.T.);
#5449=ORIENTED_EDGE('',*,*,#4343,.T.);
#5450=ORIENTED_EDGE('',*,*,#4358,.F.);
#5451=ORIENTED_EDGE('',*,*,#4359,.T.);
#5452=ORIENTED_EDGE('',*,*,#4360,.F.);
#5453=ORIENTED_EDGE('',*,*,#4359,.F.);
#5454=ORIENTED_EDGE('',*,*,#4358,.T.);
#5455=ORIENTED_EDGE('',*,*,#4361,.F.);
#5456=ORIENTED_EDGE('',*,*,#4362,.T.);
#5457=ORIENTED_EDGE('',*,*,#4363,.F.);
#5458=ORIENTED_EDGE('',*,*,#4362,.F.);
#5459=ORIENTED_EDGE('',*,*,#4361,.T.);
#5460=ORIENTED_EDGE('',*,*,#4364,.F.);
#5461=ORIENTED_EDGE('',*,*,#4365,.F.);
#5462=ORIENTED_EDGE('',*,*,#4366,.T.);
#5463=ORIENTED_EDGE('',*,*,#4364,.T.);
#5464=ORIENTED_EDGE('',*,*,#4366,.F.);
#5465=ORIENTED_EDGE('',*,*,#4367,.T.);
#5466=ORIENTED_EDGE('',*,*,#4368,.T.);
#5467=ORIENTED_EDGE('',*,*,#4369,.F.);
#5468=ORIENTED_EDGE('',*,*,#4370,.F.);
#5469=ORIENTED_EDGE('',*,*,#4360,.T.);
#5470=ORIENTED_EDGE('',*,*,#4363,.T.);
#5471=ORIENTED_EDGE('',*,*,#4371,.T.);
#5472=ORIENTED_EDGE('',*,*,#4370,.T.);
#5473=ORIENTED_EDGE('',*,*,#4372,.F.);
#5474=ORIENTED_EDGE('',*,*,#4373,.F.);
#5475=ORIENTED_EDGE('',*,*,#4374,.T.);
#5476=ORIENTED_EDGE('',*,*,#4373,.T.);
#5477=ORIENTED_EDGE('',*,*,#4375,.F.);
#5478=ORIENTED_EDGE('',*,*,#4376,.F.);
#5479=ORIENTED_EDGE('',*,*,#4365,.T.);
#5480=ORIENTED_EDGE('',*,*,#4377,.T.);
#5481=ORIENTED_EDGE('',*,*,#4376,.T.);
#5482=ORIENTED_EDGE('',*,*,#4378,.F.);
#5483=ORIENTED_EDGE('',*,*,#4368,.F.);
#5484=ORIENTED_EDGE('',*,*,#4378,.T.);
#5485=ORIENTED_EDGE('',*,*,#4375,.T.);
#5486=ORIENTED_EDGE('',*,*,#4372,.T.);
#5487=ORIENTED_EDGE('',*,*,#4369,.T.);
#5488=ORIENTED_EDGE('',*,*,#4377,.F.);
#5489=ORIENTED_EDGE('',*,*,#4367,.F.);
#5490=ORIENTED_EDGE('',*,*,#4371,.F.);
#5491=ORIENTED_EDGE('',*,*,#4374,.F.);
#5492=ORIENTED_EDGE('',*,*,#4379,.F.);
#5493=ORIENTED_EDGE('',*,*,#4380,.T.);
#5494=ORIENTED_EDGE('',*,*,#4381,.T.);
#5495=ORIENTED_EDGE('',*,*,#4380,.F.);
#5496=ORIENTED_EDGE('',*,*,#4381,.F.);
#5497=ORIENTED_EDGE('',*,*,#4382,.F.);
#5498=ORIENTED_EDGE('',*,*,#4383,.T.);
#5499=ORIENTED_EDGE('',*,*,#4384,.T.);
#5500=ORIENTED_EDGE('',*,*,#4383,.F.);
#5501=ORIENTED_EDGE('',*,*,#4384,.F.);
#5502=ORIENTED_EDGE('',*,*,#4385,.F.);
#5503=ORIENTED_EDGE('',*,*,#4385,.T.);
#5504=ORIENTED_EDGE('',*,*,#4386,.T.);
#5505=ORIENTED_EDGE('',*,*,#4387,.F.);
#5506=ORIENTED_EDGE('',*,*,#4386,.F.);
#5507=ORIENTED_EDGE('',*,*,#4388,.T.);
#5508=ORIENTED_EDGE('',*,*,#4389,.T.);
#5509=ORIENTED_EDGE('',*,*,#4390,.F.);
#5510=ORIENTED_EDGE('',*,*,#4391,.F.);
#5511=ORIENTED_EDGE('',*,*,#4387,.T.);
#5512=ORIENTED_EDGE('',*,*,#4392,.T.);
#5513=ORIENTED_EDGE('',*,*,#4391,.T.);
#5514=ORIENTED_EDGE('',*,*,#4393,.F.);
#5515=ORIENTED_EDGE('',*,*,#4394,.F.);
#5516=ORIENTED_EDGE('',*,*,#4395,.T.);
#5517=ORIENTED_EDGE('',*,*,#4394,.T.);
#5518=ORIENTED_EDGE('',*,*,#4396,.F.);
#5519=ORIENTED_EDGE('',*,*,#4397,.F.);
#5520=ORIENTED_EDGE('',*,*,#4379,.T.);
#5521=ORIENTED_EDGE('',*,*,#4382,.T.);
#5522=ORIENTED_EDGE('',*,*,#4398,.T.);
#5523=ORIENTED_EDGE('',*,*,#4397,.T.);
#5524=ORIENTED_EDGE('',*,*,#4399,.F.);
#5525=ORIENTED_EDGE('',*,*,#4389,.F.);
#5526=ORIENTED_EDGE('',*,*,#4399,.T.);
#5527=ORIENTED_EDGE('',*,*,#4396,.T.);
#5528=ORIENTED_EDGE('',*,*,#4393,.T.);
#5529=ORIENTED_EDGE('',*,*,#4390,.T.);
#5530=ORIENTED_EDGE('',*,*,#4398,.F.);
#5531=ORIENTED_EDGE('',*,*,#4388,.F.);
#5532=ORIENTED_EDGE('',*,*,#4392,.F.);
#5533=ORIENTED_EDGE('',*,*,#4395,.F.);
#5534=ORIENTED_EDGE('',*,*,#4400,.F.);
#5535=ORIENTED_EDGE('',*,*,#4401,.T.);
#5536=ORIENTED_EDGE('',*,*,#4402,.F.);
#5537=ORIENTED_EDGE('',*,*,#4401,.F.);
#5538=ORIENTED_EDGE('',*,*,#4400,.T.);
#5539=ORIENTED_EDGE('',*,*,#4403,.F.);
#5540=ORIENTED_EDGE('',*,*,#4404,.T.);
#5541=ORIENTED_EDGE('',*,*,#4405,.F.);
#5542=ORIENTED_EDGE('',*,*,#4404,.F.);
#5543=ORIENTED_EDGE('',*,*,#4403,.T.);
#5544=ORIENTED_EDGE('',*,*,#4406,.F.);
#5545=ORIENTED_EDGE('',*,*,#4407,.F.);
#5546=ORIENTED_EDGE('',*,*,#4408,.T.);
#5547=ORIENTED_EDGE('',*,*,#4406,.T.);
#5548=ORIENTED_EDGE('',*,*,#4408,.F.);
#5549=ORIENTED_EDGE('',*,*,#4409,.T.);
#5550=ORIENTED_EDGE('',*,*,#4410,.T.);
#5551=ORIENTED_EDGE('',*,*,#4411,.F.);
#5552=ORIENTED_EDGE('',*,*,#4412,.F.);
#5553=ORIENTED_EDGE('',*,*,#4402,.T.);
#5554=ORIENTED_EDGE('',*,*,#4405,.T.);
#5555=ORIENTED_EDGE('',*,*,#4413,.T.);
#5556=ORIENTED_EDGE('',*,*,#4412,.T.);
#5557=ORIENTED_EDGE('',*,*,#4414,.F.);
#5558=ORIENTED_EDGE('',*,*,#4415,.F.);
#5559=ORIENTED_EDGE('',*,*,#4416,.T.);
#5560=ORIENTED_EDGE('',*,*,#4415,.T.);
#5561=ORIENTED_EDGE('',*,*,#4417,.F.);
#5562=ORIENTED_EDGE('',*,*,#4418,.F.);
#5563=ORIENTED_EDGE('',*,*,#4407,.T.);
#5564=ORIENTED_EDGE('',*,*,#4419,.T.);
#5565=ORIENTED_EDGE('',*,*,#4418,.T.);
#5566=ORIENTED_EDGE('',*,*,#4420,.F.);
#5567=ORIENTED_EDGE('',*,*,#4410,.F.);
#5568=ORIENTED_EDGE('',*,*,#4420,.T.);
#5569=ORIENTED_EDGE('',*,*,#4417,.T.);
#5570=ORIENTED_EDGE('',*,*,#4414,.T.);
#5571=ORIENTED_EDGE('',*,*,#4411,.T.);
#5572=ORIENTED_EDGE('',*,*,#4419,.F.);
#5573=ORIENTED_EDGE('',*,*,#4409,.F.);
#5574=ORIENTED_EDGE('',*,*,#4413,.F.);
#5575=ORIENTED_EDGE('',*,*,#4416,.F.);
#5576=ORIENTED_EDGE('',*,*,#4421,.F.);
#5577=ORIENTED_EDGE('',*,*,#4422,.T.);
#5578=ORIENTED_EDGE('',*,*,#4423,.T.);
#5579=ORIENTED_EDGE('',*,*,#4422,.F.);
#5580=ORIENTED_EDGE('',*,*,#4423,.F.);
#5581=ORIENTED_EDGE('',*,*,#4424,.F.);
#5582=ORIENTED_EDGE('',*,*,#4425,.T.);
#5583=ORIENTED_EDGE('',*,*,#4426,.T.);
#5584=ORIENTED_EDGE('',*,*,#4425,.F.);
#5585=ORIENTED_EDGE('',*,*,#4426,.F.);
#5586=ORIENTED_EDGE('',*,*,#4427,.F.);
#5587=ORIENTED_EDGE('',*,*,#4427,.T.);
#5588=ORIENTED_EDGE('',*,*,#4428,.T.);
#5589=ORIENTED_EDGE('',*,*,#4429,.F.);
#5590=ORIENTED_EDGE('',*,*,#4428,.F.);
#5591=ORIENTED_EDGE('',*,*,#4430,.T.);
#5592=ORIENTED_EDGE('',*,*,#4431,.T.);
#5593=ORIENTED_EDGE('',*,*,#4432,.F.);
#5594=ORIENTED_EDGE('',*,*,#4433,.F.);
#5595=ORIENTED_EDGE('',*,*,#4429,.T.);
#5596=ORIENTED_EDGE('',*,*,#4434,.T.);
#5597=ORIENTED_EDGE('',*,*,#4433,.T.);
#5598=ORIENTED_EDGE('',*,*,#4435,.F.);
#5599=ORIENTED_EDGE('',*,*,#4436,.F.);
#5600=ORIENTED_EDGE('',*,*,#4437,.T.);
#5601=ORIENTED_EDGE('',*,*,#4436,.T.);
#5602=ORIENTED_EDGE('',*,*,#4438,.F.);
#5603=ORIENTED_EDGE('',*,*,#4439,.F.);
#5604=ORIENTED_EDGE('',*,*,#4421,.T.);
#5605=ORIENTED_EDGE('',*,*,#4424,.T.);
#5606=ORIENTED_EDGE('',*,*,#4440,.T.);
#5607=ORIENTED_EDGE('',*,*,#4439,.T.);
#5608=ORIENTED_EDGE('',*,*,#4441,.F.);
#5609=ORIENTED_EDGE('',*,*,#4431,.F.);
#5610=ORIENTED_EDGE('',*,*,#4441,.T.);
#5611=ORIENTED_EDGE('',*,*,#4438,.T.);
#5612=ORIENTED_EDGE('',*,*,#4435,.T.);
#5613=ORIENTED_EDGE('',*,*,#4432,.T.);
#5614=ORIENTED_EDGE('',*,*,#4440,.F.);
#5615=ORIENTED_EDGE('',*,*,#4430,.F.);
#5616=ORIENTED_EDGE('',*,*,#4434,.F.);
#5617=ORIENTED_EDGE('',*,*,#4437,.F.);
#5618=ORIENTED_EDGE('',*,*,#4442,.F.);
#5619=ORIENTED_EDGE('',*,*,#4443,.F.);
#5620=ORIENTED_EDGE('',*,*,#4444,.F.);
#5621=ORIENTED_EDGE('',*,*,#4445,.T.);
#5622=ORIENTED_EDGE('',*,*,#4446,.F.);
#5623=ORIENTED_EDGE('',*,*,#4445,.F.);
#5624=ORIENTED_EDGE('',*,*,#4447,.F.);
#5625=ORIENTED_EDGE('',*,*,#4448,.T.);
#5626=ORIENTED_EDGE('',*,*,#4449,.F.);
#5627=ORIENTED_EDGE('',*,*,#4448,.F.);
#5628=ORIENTED_EDGE('',*,*,#4450,.F.);
#5629=ORIENTED_EDGE('',*,*,#4451,.T.);
#5630=ORIENTED_EDGE('',*,*,#4452,.F.);
#5631=ORIENTED_EDGE('',*,*,#4451,.F.);
#5632=ORIENTED_EDGE('',*,*,#4453,.F.);
#5633=ORIENTED_EDGE('',*,*,#4443,.T.);
#5634=ORIENTED_EDGE('',*,*,#4454,.T.);
#5635=ORIENTED_EDGE('',*,*,#4455,.T.);
#5636=ORIENTED_EDGE('',*,*,#4456,.F.);
#5637=ORIENTED_EDGE('',*,*,#4457,.F.);
#5638=ORIENTED_EDGE('',*,*,#4458,.T.);
#5639=ORIENTED_EDGE('',*,*,#4457,.T.);
#5640=ORIENTED_EDGE('',*,*,#4459,.F.);
#5641=ORIENTED_EDGE('',*,*,#4460,.F.);
#5642=ORIENTED_EDGE('',*,*,#4461,.T.);
#5643=ORIENTED_EDGE('',*,*,#4460,.T.);
#5644=ORIENTED_EDGE('',*,*,#4462,.F.);
#5645=ORIENTED_EDGE('',*,*,#4463,.F.);
#5646=ORIENTED_EDGE('',*,*,#4464,.T.);
#5647=ORIENTED_EDGE('',*,*,#4463,.T.);
#5648=ORIENTED_EDGE('',*,*,#4465,.F.);
#5649=ORIENTED_EDGE('',*,*,#4455,.F.);
#5650=ORIENTED_EDGE('',*,*,#4465,.T.);
#5651=ORIENTED_EDGE('',*,*,#4462,.T.);
#5652=ORIENTED_EDGE('',*,*,#4459,.T.);
#5653=ORIENTED_EDGE('',*,*,#4456,.T.);
#5654=ORIENTED_EDGE('',*,*,#4449,.T.);
#5655=ORIENTED_EDGE('',*,*,#4452,.T.);
#5656=ORIENTED_EDGE('',*,*,#4442,.T.);
#5657=ORIENTED_EDGE('',*,*,#4446,.T.);
#5658=ORIENTED_EDGE('',*,*,#4464,.F.);
#5659=ORIENTED_EDGE('',*,*,#4454,.F.);
#5660=ORIENTED_EDGE('',*,*,#4458,.F.);
#5661=ORIENTED_EDGE('',*,*,#4461,.F.);
#5662=ORIENTED_EDGE('',*,*,#4450,.T.);
#5663=ORIENTED_EDGE('',*,*,#4447,.T.);
#5664=ORIENTED_EDGE('',*,*,#4444,.T.);
#5665=ORIENTED_EDGE('',*,*,#4453,.T.);
#5666=ORIENTED_EDGE('',*,*,#4466,.F.);
#5667=ORIENTED_EDGE('',*,*,#4467,.F.);
#5668=ORIENTED_EDGE('',*,*,#4468,.F.);
#5669=ORIENTED_EDGE('',*,*,#4469,.T.);
#5670=ORIENTED_EDGE('',*,*,#4470,.F.);
#5671=ORIENTED_EDGE('',*,*,#4469,.F.);
#5672=ORIENTED_EDGE('',*,*,#4471,.F.);
#5673=ORIENTED_EDGE('',*,*,#4472,.T.);
#5674=ORIENTED_EDGE('',*,*,#4473,.F.);
#5675=ORIENTED_EDGE('',*,*,#4472,.F.);
#5676=ORIENTED_EDGE('',*,*,#4474,.F.);
#5677=ORIENTED_EDGE('',*,*,#4475,.T.);
#5678=ORIENTED_EDGE('',*,*,#4476,.F.);
#5679=ORIENTED_EDGE('',*,*,#4475,.F.);
#5680=ORIENTED_EDGE('',*,*,#4477,.F.);
#5681=ORIENTED_EDGE('',*,*,#4467,.T.);
#5682=ORIENTED_EDGE('',*,*,#4478,.T.);
#5683=ORIENTED_EDGE('',*,*,#4479,.T.);
#5684=ORIENTED_EDGE('',*,*,#4480,.F.);
#5685=ORIENTED_EDGE('',*,*,#4481,.F.);
#5686=ORIENTED_EDGE('',*,*,#4482,.T.);
#5687=ORIENTED_EDGE('',*,*,#4481,.T.);
#5688=ORIENTED_EDGE('',*,*,#4483,.F.);
#5689=ORIENTED_EDGE('',*,*,#4484,.F.);
#5690=ORIENTED_EDGE('',*,*,#4485,.T.);
#5691=ORIENTED_EDGE('',*,*,#4484,.T.);
#5692=ORIENTED_EDGE('',*,*,#4486,.F.);
#5693=ORIENTED_EDGE('',*,*,#4487,.F.);
#5694=ORIENTED_EDGE('',*,*,#4488,.T.);
#5695=ORIENTED_EDGE('',*,*,#4487,.T.);
#5696=ORIENTED_EDGE('',*,*,#4489,.F.);
#5697=ORIENTED_EDGE('',*,*,#4479,.F.);
#5698=ORIENTED_EDGE('',*,*,#4489,.T.);
#5699=ORIENTED_EDGE('',*,*,#4486,.T.);
#5700=ORIENTED_EDGE('',*,*,#4483,.T.);
#5701=ORIENTED_EDGE('',*,*,#4480,.T.);
#5702=ORIENTED_EDGE('',*,*,#4473,.T.);
#5703=ORIENTED_EDGE('',*,*,#4476,.T.);
#5704=ORIENTED_EDGE('',*,*,#4466,.T.);
#5705=ORIENTED_EDGE('',*,*,#4470,.T.);
#5706=ORIENTED_EDGE('',*,*,#4488,.F.);
#5707=ORIENTED_EDGE('',*,*,#4478,.F.);
#5708=ORIENTED_EDGE('',*,*,#4482,.F.);
#5709=ORIENTED_EDGE('',*,*,#4485,.F.);
#5710=ORIENTED_EDGE('',*,*,#4474,.T.);
#5711=ORIENTED_EDGE('',*,*,#4471,.T.);
#5712=ORIENTED_EDGE('',*,*,#4468,.T.);
#5713=ORIENTED_EDGE('',*,*,#4477,.T.);
#5714=ORIENTED_EDGE('',*,*,#4490,.F.);
#5715=ORIENTED_EDGE('',*,*,#4491,.T.);
#5716=ORIENTED_EDGE('',*,*,#4492,.F.);
#5717=ORIENTED_EDGE('',*,*,#4491,.F.);
#5718=ORIENTED_EDGE('',*,*,#4493,.F.);
#5719=ORIENTED_EDGE('',*,*,#4494,.T.);
#5720=ORIENTED_EDGE('',*,*,#4495,.F.);
#5721=ORIENTED_EDGE('',*,*,#4494,.F.);
#5722=ORIENTED_EDGE('',*,*,#4496,.F.);
#5723=ORIENTED_EDGE('',*,*,#4497,.T.);
#5724=ORIENTED_EDGE('',*,*,#4498,.F.);
#5725=ORIENTED_EDGE('',*,*,#4497,.F.);
#5726=ORIENTED_EDGE('',*,*,#4499,.F.);
#5727=ORIENTED_EDGE('',*,*,#4500,.T.);
#5728=ORIENTED_EDGE('',*,*,#4501,.F.);
#5729=ORIENTED_EDGE('',*,*,#4500,.F.);
#5730=ORIENTED_EDGE('',*,*,#4502,.F.);
#5731=ORIENTED_EDGE('',*,*,#4503,.T.);
#5732=ORIENTED_EDGE('',*,*,#4504,.F.);
#5733=ORIENTED_EDGE('',*,*,#4503,.F.);
#5734=ORIENTED_EDGE('',*,*,#4505,.F.);
#5735=ORIENTED_EDGE('',*,*,#4506,.T.);
#5736=ORIENTED_EDGE('',*,*,#4507,.F.);
#5737=ORIENTED_EDGE('',*,*,#4506,.F.);
#5738=ORIENTED_EDGE('',*,*,#4508,.F.);
#5739=ORIENTED_EDGE('',*,*,#4509,.T.);
#5740=ORIENTED_EDGE('',*,*,#4510,.F.);
#5741=ORIENTED_EDGE('',*,*,#4509,.F.);
#5742=ORIENTED_EDGE('',*,*,#4511,.F.);
#5743=ORIENTED_EDGE('',*,*,#4512,.T.);
#5744=ORIENTED_EDGE('',*,*,#4513,.F.);
#5745=ORIENTED_EDGE('',*,*,#4512,.F.);
#5746=ORIENTED_EDGE('',*,*,#4514,.T.);
#5747=ORIENTED_EDGE('',*,*,#4515,.T.);
#5748=ORIENTED_EDGE('',*,*,#4516,.F.);
#5749=ORIENTED_EDGE('',*,*,#4517,.F.);
#5750=ORIENTED_EDGE('',*,*,#4518,.T.);
#5751=ORIENTED_EDGE('',*,*,#4517,.T.);
#5752=ORIENTED_EDGE('',*,*,#4519,.F.);
#5753=ORIENTED_EDGE('',*,*,#4520,.F.);
#5754=ORIENTED_EDGE('',*,*,#4498,.T.);
#5755=ORIENTED_EDGE('',*,*,#4501,.T.);
#5756=ORIENTED_EDGE('',*,*,#4504,.T.);
#5757=ORIENTED_EDGE('',*,*,#4507,.T.);
#5758=ORIENTED_EDGE('',*,*,#4510,.T.);
#5759=ORIENTED_EDGE('',*,*,#4513,.T.);
#5760=ORIENTED_EDGE('',*,*,#4495,.T.);
#5761=ORIENTED_EDGE('',*,*,#4492,.T.);
#5762=ORIENTED_EDGE('',*,*,#4521,.T.);
#5763=ORIENTED_EDGE('',*,*,#4520,.T.);
#5764=ORIENTED_EDGE('',*,*,#4522,.F.);
#5765=ORIENTED_EDGE('',*,*,#4523,.F.);
#5766=ORIENTED_EDGE('',*,*,#4524,.T.);
#5767=ORIENTED_EDGE('',*,*,#4523,.T.);
#5768=ORIENTED_EDGE('',*,*,#4525,.F.);
#5769=ORIENTED_EDGE('',*,*,#4515,.F.);
#5770=ORIENTED_EDGE('',*,*,#4496,.T.);
#5771=ORIENTED_EDGE('',*,*,#4499,.T.);
#5772=ORIENTED_EDGE('',*,*,#4502,.T.);
#5773=ORIENTED_EDGE('',*,*,#4505,.T.);
#5774=ORIENTED_EDGE('',*,*,#4508,.T.);
#5775=ORIENTED_EDGE('',*,*,#4511,.T.);
#5776=ORIENTED_EDGE('',*,*,#4493,.T.);
#5777=ORIENTED_EDGE('',*,*,#4490,.T.);
#5778=ORIENTED_EDGE('',*,*,#4525,.T.);
#5779=ORIENTED_EDGE('',*,*,#4522,.T.);
#5780=ORIENTED_EDGE('',*,*,#4519,.T.);
#5781=ORIENTED_EDGE('',*,*,#4516,.T.);
#5782=ORIENTED_EDGE('',*,*,#4524,.F.);
#5783=ORIENTED_EDGE('',*,*,#4514,.F.);
#5784=ORIENTED_EDGE('',*,*,#4518,.F.);
#5785=ORIENTED_EDGE('',*,*,#4521,.F.);
#5786=ORIENTED_EDGE('',*,*,#4526,.F.);
#5787=ORIENTED_EDGE('',*,*,#4527,.T.);
#5788=ORIENTED_EDGE('',*,*,#4528,.F.);
#5789=ORIENTED_EDGE('',*,*,#4527,.F.);
#5790=ORIENTED_EDGE('',*,*,#4529,.F.);
#5791=ORIENTED_EDGE('',*,*,#4530,.T.);
#5792=ORIENTED_EDGE('',*,*,#4531,.F.);
#5793=ORIENTED_EDGE('',*,*,#4530,.F.);
#5794=ORIENTED_EDGE('',*,*,#4532,.T.);
#5795=ORIENTED_EDGE('',*,*,#4533,.T.);
#5796=ORIENTED_EDGE('',*,*,#4534,.F.);
#5797=ORIENTED_EDGE('',*,*,#4535,.F.);
#5798=ORIENTED_EDGE('',*,*,#4536,.T.);
#5799=ORIENTED_EDGE('',*,*,#4535,.T.);
#5800=ORIENTED_EDGE('',*,*,#4537,.F.);
#5801=ORIENTED_EDGE('',*,*,#4538,.F.);
#5802=ORIENTED_EDGE('',*,*,#4539,.T.);
#5803=ORIENTED_EDGE('',*,*,#4538,.T.);
#5804=ORIENTED_EDGE('',*,*,#4540,.F.);
#5805=ORIENTED_EDGE('',*,*,#4541,.F.);
#5806=ORIENTED_EDGE('',*,*,#4542,.T.);
#5807=ORIENTED_EDGE('',*,*,#4541,.T.);
#5808=ORIENTED_EDGE('',*,*,#4543,.F.);
#5809=ORIENTED_EDGE('',*,*,#4544,.F.);
#5810=ORIENTED_EDGE('',*,*,#4528,.T.);
#5811=ORIENTED_EDGE('',*,*,#4531,.T.);
#5812=ORIENTED_EDGE('',*,*,#4545,.T.);
#5813=ORIENTED_EDGE('',*,*,#4544,.T.);
#5814=ORIENTED_EDGE('',*,*,#4546,.F.);
#5815=ORIENTED_EDGE('',*,*,#4547,.F.);
#5816=ORIENTED_EDGE('',*,*,#4548,.T.);
#5817=ORIENTED_EDGE('',*,*,#4547,.T.);
#5818=ORIENTED_EDGE('',*,*,#4549,.F.);
#5819=ORIENTED_EDGE('',*,*,#4533,.F.);
#5820=ORIENTED_EDGE('',*,*,#4526,.T.);
#5821=ORIENTED_EDGE('',*,*,#4529,.T.);
#5822=ORIENTED_EDGE('',*,*,#4549,.T.);
#5823=ORIENTED_EDGE('',*,*,#4546,.T.);
#5824=ORIENTED_EDGE('',*,*,#4543,.T.);
#5825=ORIENTED_EDGE('',*,*,#4540,.T.);
#5826=ORIENTED_EDGE('',*,*,#4537,.T.);
#5827=ORIENTED_EDGE('',*,*,#4534,.T.);
#5828=ORIENTED_EDGE('',*,*,#4548,.F.);
#5829=ORIENTED_EDGE('',*,*,#4532,.F.);
#5830=ORIENTED_EDGE('',*,*,#4536,.F.);
#5831=ORIENTED_EDGE('',*,*,#4539,.F.);
#5832=ORIENTED_EDGE('',*,*,#4542,.F.);
#5833=ORIENTED_EDGE('',*,*,#4545,.F.);
#5834=ORIENTED_EDGE('',*,*,#4550,.F.);
#5835=ORIENTED_EDGE('',*,*,#4551,.T.);
#5836=ORIENTED_EDGE('',*,*,#4552,.T.);
#5837=ORIENTED_EDGE('',*,*,#4551,.F.);
#5838=ORIENTED_EDGE('',*,*,#4552,.F.);
#5839=ORIENTED_EDGE('',*,*,#4553,.F.);
#5840=ORIENTED_EDGE('',*,*,#4554,.T.);
#5841=ORIENTED_EDGE('',*,*,#4555,.F.);
#5842=ORIENTED_EDGE('',*,*,#4554,.F.);
#5843=ORIENTED_EDGE('',*,*,#4556,.F.);
#5844=ORIENTED_EDGE('',*,*,#4557,.F.);
#5845=ORIENTED_EDGE('',*,*,#4558,.F.);
#5846=ORIENTED_EDGE('',*,*,#4559,.F.);
#5847=ORIENTED_EDGE('',*,*,#4560,.F.);
#5848=ORIENTED_EDGE('',*,*,#4558,.T.);
#5849=ORIENTED_EDGE('',*,*,#4561,.F.);
#5850=ORIENTED_EDGE('',*,*,#4562,.F.);
#5851=ORIENTED_EDGE('',*,*,#4550,.T.);
#5852=ORIENTED_EDGE('',*,*,#4563,.F.);
#5853=ORIENTED_EDGE('',*,*,#4559,.T.);
#5854=ORIENTED_EDGE('',*,*,#4560,.T.);
#5855=ORIENTED_EDGE('',*,*,#4564,.T.);
#5856=ORIENTED_EDGE('',*,*,#4565,.T.);
#5857=ORIENTED_EDGE('',*,*,#4566,.F.);
#5858=ORIENTED_EDGE('',*,*,#4567,.F.);
#5859=ORIENTED_EDGE('',*,*,#4568,.T.);
#5860=ORIENTED_EDGE('',*,*,#4561,.T.);
#5861=ORIENTED_EDGE('',*,*,#4557,.T.);
#5862=ORIENTED_EDGE('',*,*,#4569,.F.);
#5863=ORIENTED_EDGE('',*,*,#4570,.F.);
#5864=ORIENTED_EDGE('',*,*,#4571,.F.);
#5865=ORIENTED_EDGE('',*,*,#4564,.F.);
#5866=ORIENTED_EDGE('',*,*,#4562,.T.);
#5867=ORIENTED_EDGE('',*,*,#4568,.F.);
#5868=ORIENTED_EDGE('',*,*,#4567,.T.);
#5869=ORIENTED_EDGE('',*,*,#4572,.F.);
#5870=ORIENTED_EDGE('',*,*,#4573,.F.);
#5871=ORIENTED_EDGE('',*,*,#4569,.T.);
#5872=ORIENTED_EDGE('',*,*,#4555,.T.);
#5873=ORIENTED_EDGE('',*,*,#4570,.T.);
#5874=ORIENTED_EDGE('',*,*,#4573,.T.);
#5875=ORIENTED_EDGE('',*,*,#4574,.F.);
#5876=ORIENTED_EDGE('',*,*,#4575,.F.);
#5877=ORIENTED_EDGE('',*,*,#4563,.T.);
#5878=ORIENTED_EDGE('',*,*,#4571,.T.);
#5879=ORIENTED_EDGE('',*,*,#4575,.T.);
#5880=ORIENTED_EDGE('',*,*,#4576,.F.);
#5881=ORIENTED_EDGE('',*,*,#4565,.F.);
#5882=ORIENTED_EDGE('',*,*,#4556,.T.);
#5883=ORIENTED_EDGE('',*,*,#4553,.T.);
#5884=ORIENTED_EDGE('',*,*,#4576,.T.);
#5885=ORIENTED_EDGE('',*,*,#4574,.T.);
#5886=ORIENTED_EDGE('',*,*,#4572,.T.);
#5887=ORIENTED_EDGE('',*,*,#4566,.T.);
#5888=ORIENTED_EDGE('',*,*,#4577,.F.);
#5889=ORIENTED_EDGE('',*,*,#4578,.T.);
#5890=ORIENTED_EDGE('',*,*,#4579,.T.);
#5891=ORIENTED_EDGE('',*,*,#4578,.F.);
#5892=ORIENTED_EDGE('',*,*,#4579,.F.);
#5893=ORIENTED_EDGE('',*,*,#4580,.F.);
#5894=ORIENTED_EDGE('',*,*,#4581,.T.);
#5895=ORIENTED_EDGE('',*,*,#4582,.F.);
#5896=ORIENTED_EDGE('',*,*,#4581,.F.);
#5897=ORIENTED_EDGE('',*,*,#4583,.F.);
#5898=ORIENTED_EDGE('',*,*,#4584,.F.);
#5899=ORIENTED_EDGE('',*,*,#4585,.F.);
#5900=ORIENTED_EDGE('',*,*,#4586,.F.);
#5901=ORIENTED_EDGE('',*,*,#4587,.F.);
#5902=ORIENTED_EDGE('',*,*,#4585,.T.);
#5903=ORIENTED_EDGE('',*,*,#4588,.F.);
#5904=ORIENTED_EDGE('',*,*,#4589,.F.);
#5905=ORIENTED_EDGE('',*,*,#4577,.T.);
#5906=ORIENTED_EDGE('',*,*,#4590,.F.);
#5907=ORIENTED_EDGE('',*,*,#4586,.T.);
#5908=ORIENTED_EDGE('',*,*,#4587,.T.);
#5909=ORIENTED_EDGE('',*,*,#4591,.T.);
#5910=ORIENTED_EDGE('',*,*,#4592,.T.);
#5911=ORIENTED_EDGE('',*,*,#4593,.F.);
#5912=ORIENTED_EDGE('',*,*,#4594,.F.);
#5913=ORIENTED_EDGE('',*,*,#4595,.T.);
#5914=ORIENTED_EDGE('',*,*,#4588,.T.);
#5915=ORIENTED_EDGE('',*,*,#4584,.T.);
#5916=ORIENTED_EDGE('',*,*,#4596,.F.);
#5917=ORIENTED_EDGE('',*,*,#4597,.F.);
#5918=ORIENTED_EDGE('',*,*,#4598,.F.);
#5919=ORIENTED_EDGE('',*,*,#4591,.F.);
#5920=ORIENTED_EDGE('',*,*,#4589,.T.);
#5921=ORIENTED_EDGE('',*,*,#4595,.F.);
#5922=ORIENTED_EDGE('',*,*,#4594,.T.);
#5923=ORIENTED_EDGE('',*,*,#4599,.F.);
#5924=ORIENTED_EDGE('',*,*,#4600,.F.);
#5925=ORIENTED_EDGE('',*,*,#4596,.T.);
#5926=ORIENTED_EDGE('',*,*,#4582,.T.);
#5927=ORIENTED_EDGE('',*,*,#4597,.T.);
#5928=ORIENTED_EDGE('',*,*,#4600,.T.);
#5929=ORIENTED_EDGE('',*,*,#4601,.F.);
#5930=ORIENTED_EDGE('',*,*,#4602,.F.);
#5931=ORIENTED_EDGE('',*,*,#4590,.T.);
#5932=ORIENTED_EDGE('',*,*,#4598,.T.);
#5933=ORIENTED_EDGE('',*,*,#4602,.T.);
#5934=ORIENTED_EDGE('',*,*,#4603,.F.);
#5935=ORIENTED_EDGE('',*,*,#4592,.F.);
#5936=ORIENTED_EDGE('',*,*,#4583,.T.);
#5937=ORIENTED_EDGE('',*,*,#4580,.T.);
#5938=ORIENTED_EDGE('',*,*,#4603,.T.);
#5939=ORIENTED_EDGE('',*,*,#4601,.T.);
#5940=ORIENTED_EDGE('',*,*,#4599,.T.);
#5941=ORIENTED_EDGE('',*,*,#4593,.T.);
#5942=ORIENTED_EDGE('',*,*,#4604,.F.);
#5943=ORIENTED_EDGE('',*,*,#4605,.T.);
#5944=ORIENTED_EDGE('',*,*,#4606,.F.);
#5945=ORIENTED_EDGE('',*,*,#4605,.F.);
#5946=ORIENTED_EDGE('',*,*,#4607,.T.);
#5947=ORIENTED_EDGE('',*,*,#4608,.T.);
#5948=ORIENTED_EDGE('',*,*,#4609,.F.);
#5949=ORIENTED_EDGE('',*,*,#4610,.F.);
#5950=ORIENTED_EDGE('',*,*,#4611,.T.);
#5951=ORIENTED_EDGE('',*,*,#4610,.T.);
#5952=ORIENTED_EDGE('',*,*,#4612,.F.);
#5953=ORIENTED_EDGE('',*,*,#4613,.F.);
#5954=ORIENTED_EDGE('',*,*,#4606,.T.);
#5955=ORIENTED_EDGE('',*,*,#4614,.T.);
#5956=ORIENTED_EDGE('',*,*,#4613,.T.);
#5957=ORIENTED_EDGE('',*,*,#4615,.F.);
#5958=ORIENTED_EDGE('',*,*,#4616,.F.);
#5959=ORIENTED_EDGE('',*,*,#4617,.T.);
#5960=ORIENTED_EDGE('',*,*,#4616,.T.);
#5961=ORIENTED_EDGE('',*,*,#4618,.F.);
#5962=ORIENTED_EDGE('',*,*,#4608,.F.);
#5963=ORIENTED_EDGE('',*,*,#4604,.T.);
#5964=ORIENTED_EDGE('',*,*,#4618,.T.);
#5965=ORIENTED_EDGE('',*,*,#4615,.T.);
#5966=ORIENTED_EDGE('',*,*,#4612,.T.);
#5967=ORIENTED_EDGE('',*,*,#4609,.T.);
#5968=ORIENTED_EDGE('',*,*,#4617,.F.);
#5969=ORIENTED_EDGE('',*,*,#4607,.F.);
#5970=ORIENTED_EDGE('',*,*,#4611,.F.);
#5971=ORIENTED_EDGE('',*,*,#4614,.F.);
#5972=ORIENTED_EDGE('',*,*,#4619,.F.);
#5973=ORIENTED_EDGE('',*,*,#4620,.T.);
#5974=ORIENTED_EDGE('',*,*,#4621,.F.);
#5975=ORIENTED_EDGE('',*,*,#4620,.F.);
#5976=ORIENTED_EDGE('',*,*,#4622,.T.);
#5977=ORIENTED_EDGE('',*,*,#4623,.T.);
#5978=ORIENTED_EDGE('',*,*,#4624,.F.);
#5979=ORIENTED_EDGE('',*,*,#4625,.F.);
#5980=ORIENTED_EDGE('',*,*,#4626,.T.);
#5981=ORIENTED_EDGE('',*,*,#4625,.T.);
#5982=ORIENTED_EDGE('',*,*,#4627,.F.);
#5983=ORIENTED_EDGE('',*,*,#4628,.F.);
#5984=ORIENTED_EDGE('',*,*,#4621,.T.);
#5985=ORIENTED_EDGE('',*,*,#4629,.T.);
#5986=ORIENTED_EDGE('',*,*,#4628,.T.);
#5987=ORIENTED_EDGE('',*,*,#4630,.F.);
#5988=ORIENTED_EDGE('',*,*,#4631,.F.);
#5989=ORIENTED_EDGE('',*,*,#4632,.T.);
#5990=ORIENTED_EDGE('',*,*,#4631,.T.);
#5991=ORIENTED_EDGE('',*,*,#4633,.F.);
#5992=ORIENTED_EDGE('',*,*,#4623,.F.);
#5993=ORIENTED_EDGE('',*,*,#4619,.T.);
#5994=ORIENTED_EDGE('',*,*,#4633,.T.);
#5995=ORIENTED_EDGE('',*,*,#4630,.T.);
#5996=ORIENTED_EDGE('',*,*,#4627,.T.);
#5997=ORIENTED_EDGE('',*,*,#4624,.T.);
#5998=ORIENTED_EDGE('',*,*,#4632,.F.);
#5999=ORIENTED_EDGE('',*,*,#4622,.F.);
#6000=ORIENTED_EDGE('',*,*,#4626,.F.);
#6001=ORIENTED_EDGE('',*,*,#4629,.F.);
#6002=ORIENTED_EDGE('',*,*,#4634,.F.);
#6003=ORIENTED_EDGE('',*,*,#4635,.T.);
#6004=ORIENTED_EDGE('',*,*,#4636,.F.);
#6005=ORIENTED_EDGE('',*,*,#4637,.F.);
#6006=ORIENTED_EDGE('',*,*,#4638,.F.);
#6007=ORIENTED_EDGE('',*,*,#4639,.T.);
#6008=ORIENTED_EDGE('',*,*,#4640,.F.);
#6009=ORIENTED_EDGE('',*,*,#4635,.F.);
#6010=ORIENTED_EDGE('',*,*,#4641,.F.);
#6011=ORIENTED_EDGE('',*,*,#4642,.T.);
#6012=ORIENTED_EDGE('',*,*,#4643,.F.);
#6013=ORIENTED_EDGE('',*,*,#4639,.F.);
#6014=ORIENTED_EDGE('',*,*,#4644,.F.);
#6015=ORIENTED_EDGE('',*,*,#4645,.T.);
#6016=ORIENTED_EDGE('',*,*,#4646,.F.);
#6017=ORIENTED_EDGE('',*,*,#4642,.F.);
#6018=ORIENTED_EDGE('',*,*,#4647,.F.);
#6019=ORIENTED_EDGE('',*,*,#4648,.T.);
#6020=ORIENTED_EDGE('',*,*,#4649,.F.);
#6021=ORIENTED_EDGE('',*,*,#4645,.F.);
#6022=ORIENTED_EDGE('',*,*,#4650,.F.);
#6023=ORIENTED_EDGE('',*,*,#4651,.T.);
#6024=ORIENTED_EDGE('',*,*,#4652,.F.);
#6025=ORIENTED_EDGE('',*,*,#4648,.F.);
#6026=ORIENTED_EDGE('',*,*,#4653,.F.);
#6027=ORIENTED_EDGE('',*,*,#4654,.T.);
#6028=ORIENTED_EDGE('',*,*,#4655,.F.);
#6029=ORIENTED_EDGE('',*,*,#4651,.F.);
#6030=ORIENTED_EDGE('',*,*,#4656,.F.);
#6031=ORIENTED_EDGE('',*,*,#4657,.T.);
#6032=ORIENTED_EDGE('',*,*,#4658,.F.);
#6033=ORIENTED_EDGE('',*,*,#4654,.F.);
#6034=ORIENTED_EDGE('',*,*,#4659,.F.);
#6035=ORIENTED_EDGE('',*,*,#4660,.F.);
#6036=ORIENTED_EDGE('',*,*,#4661,.F.);
#6037=ORIENTED_EDGE('',*,*,#4657,.F.);
#6038=ORIENTED_EDGE('',*,*,#4662,.F.);
#6039=ORIENTED_EDGE('',*,*,#4663,.T.);
#6040=ORIENTED_EDGE('',*,*,#4664,.F.);
#6041=ORIENTED_EDGE('',*,*,#4665,.F.);
#6042=ORIENTED_EDGE('',*,*,#4666,.F.);
#6043=ORIENTED_EDGE('',*,*,#4667,.T.);
#6044=ORIENTED_EDGE('',*,*,#4668,.F.);
#6045=ORIENTED_EDGE('',*,*,#4663,.F.);
#6046=ORIENTED_EDGE('',*,*,#4669,.F.);
#6047=ORIENTED_EDGE('',*,*,#4670,.T.);
#6048=ORIENTED_EDGE('',*,*,#4671,.F.);
#6049=ORIENTED_EDGE('',*,*,#4667,.F.);
#6050=ORIENTED_EDGE('',*,*,#4672,.F.);
#6051=ORIENTED_EDGE('',*,*,#4673,.T.);
#6052=ORIENTED_EDGE('',*,*,#4674,.F.);
#6053=ORIENTED_EDGE('',*,*,#4670,.F.);
#6054=ORIENTED_EDGE('',*,*,#4675,.F.);
#6055=ORIENTED_EDGE('',*,*,#4676,.T.);
#6056=ORIENTED_EDGE('',*,*,#4677,.F.);
#6057=ORIENTED_EDGE('',*,*,#4673,.F.);
#6058=ORIENTED_EDGE('',*,*,#4678,.F.);
#6059=ORIENTED_EDGE('',*,*,#4679,.T.);
#6060=ORIENTED_EDGE('',*,*,#4680,.F.);
#6061=ORIENTED_EDGE('',*,*,#4676,.F.);
#6062=ORIENTED_EDGE('',*,*,#4681,.F.);
#6063=ORIENTED_EDGE('',*,*,#4682,.T.);
#6064=ORIENTED_EDGE('',*,*,#4683,.F.);
#6065=ORIENTED_EDGE('',*,*,#4679,.F.);
#6066=ORIENTED_EDGE('',*,*,#4684,.F.);
#6067=ORIENTED_EDGE('',*,*,#4685,.T.);
#6068=ORIENTED_EDGE('',*,*,#4686,.F.);
#6069=ORIENTED_EDGE('',*,*,#4682,.F.);
#6070=ORIENTED_EDGE('',*,*,#4687,.F.);
#6071=ORIENTED_EDGE('',*,*,#4688,.F.);
#6072=ORIENTED_EDGE('',*,*,#4689,.F.);
#6073=ORIENTED_EDGE('',*,*,#4685,.F.);
#6074=ORIENTED_EDGE('',*,*,#4690,.F.);
#6075=ORIENTED_EDGE('',*,*,#4691,.T.);
#6076=ORIENTED_EDGE('',*,*,#4692,.F.);
#6077=ORIENTED_EDGE('',*,*,#4693,.F.);
#6078=ORIENTED_EDGE('',*,*,#4694,.F.);
#6079=ORIENTED_EDGE('',*,*,#4695,.T.);
#6080=ORIENTED_EDGE('',*,*,#4696,.F.);
#6081=ORIENTED_EDGE('',*,*,#4691,.F.);
#6082=ORIENTED_EDGE('',*,*,#4697,.F.);
#6083=ORIENTED_EDGE('',*,*,#4698,.T.);
#6084=ORIENTED_EDGE('',*,*,#4699,.F.);
#6085=ORIENTED_EDGE('',*,*,#4695,.F.);
#6086=ORIENTED_EDGE('',*,*,#4700,.F.);
#6087=ORIENTED_EDGE('',*,*,#4701,.T.);
#6088=ORIENTED_EDGE('',*,*,#4702,.F.);
#6089=ORIENTED_EDGE('',*,*,#4698,.F.);
#6090=ORIENTED_EDGE('',*,*,#4703,.F.);
#6091=ORIENTED_EDGE('',*,*,#4704,.T.);
#6092=ORIENTED_EDGE('',*,*,#4705,.F.);
#6093=ORIENTED_EDGE('',*,*,#4701,.F.);
#6094=ORIENTED_EDGE('',*,*,#4706,.F.);
#6095=ORIENTED_EDGE('',*,*,#4707,.T.);
#6096=ORIENTED_EDGE('',*,*,#4708,.F.);
#6097=ORIENTED_EDGE('',*,*,#4704,.F.);
#6098=ORIENTED_EDGE('',*,*,#4709,.F.);
#6099=ORIENTED_EDGE('',*,*,#4710,.T.);
#6100=ORIENTED_EDGE('',*,*,#4711,.F.);
#6101=ORIENTED_EDGE('',*,*,#4707,.F.);
#6102=ORIENTED_EDGE('',*,*,#4712,.F.);
#6103=ORIENTED_EDGE('',*,*,#4713,.T.);
#6104=ORIENTED_EDGE('',*,*,#4714,.F.);
#6105=ORIENTED_EDGE('',*,*,#4710,.F.);
#6106=ORIENTED_EDGE('',*,*,#4715,.F.);
#6107=ORIENTED_EDGE('',*,*,#4716,.F.);
#6108=ORIENTED_EDGE('',*,*,#4717,.F.);
#6109=ORIENTED_EDGE('',*,*,#4713,.F.);
#6110=ORIENTED_EDGE('',*,*,#4718,.F.);
#6111=ORIENTED_EDGE('',*,*,#4719,.T.);
#6112=ORIENTED_EDGE('',*,*,#4720,.F.);
#6113=ORIENTED_EDGE('',*,*,#4721,.F.);
#6114=ORIENTED_EDGE('',*,*,#4722,.F.);
#6115=ORIENTED_EDGE('',*,*,#4723,.T.);
#6116=ORIENTED_EDGE('',*,*,#4724,.F.);
#6117=ORIENTED_EDGE('',*,*,#4719,.F.);
#6118=ORIENTED_EDGE('',*,*,#4725,.F.);
#6119=ORIENTED_EDGE('',*,*,#4726,.T.);
#6120=ORIENTED_EDGE('',*,*,#4727,.F.);
#6121=ORIENTED_EDGE('',*,*,#4723,.F.);
#6122=ORIENTED_EDGE('',*,*,#4728,.F.);
#6123=ORIENTED_EDGE('',*,*,#4729,.T.);
#6124=ORIENTED_EDGE('',*,*,#4730,.F.);
#6125=ORIENTED_EDGE('',*,*,#4726,.F.);
#6126=ORIENTED_EDGE('',*,*,#4731,.F.);
#6127=ORIENTED_EDGE('',*,*,#4732,.T.);
#6128=ORIENTED_EDGE('',*,*,#4733,.F.);
#6129=ORIENTED_EDGE('',*,*,#4729,.F.);
#6130=ORIENTED_EDGE('',*,*,#4734,.F.);
#6131=ORIENTED_EDGE('',*,*,#4735,.T.);
#6132=ORIENTED_EDGE('',*,*,#4736,.F.);
#6133=ORIENTED_EDGE('',*,*,#4732,.F.);
#6134=ORIENTED_EDGE('',*,*,#4737,.F.);
#6135=ORIENTED_EDGE('',*,*,#4738,.T.);
#6136=ORIENTED_EDGE('',*,*,#4739,.F.);
#6137=ORIENTED_EDGE('',*,*,#4735,.F.);
#6138=ORIENTED_EDGE('',*,*,#4740,.F.);
#6139=ORIENTED_EDGE('',*,*,#4741,.T.);
#6140=ORIENTED_EDGE('',*,*,#4742,.F.);
#6141=ORIENTED_EDGE('',*,*,#4738,.F.);
#6142=ORIENTED_EDGE('',*,*,#4743,.F.);
#6143=ORIENTED_EDGE('',*,*,#4744,.F.);
#6144=ORIENTED_EDGE('',*,*,#4745,.F.);
#6145=ORIENTED_EDGE('',*,*,#4741,.F.);
#6146=ORIENTED_EDGE('',*,*,#4746,.F.);
#6147=ORIENTED_EDGE('',*,*,#4747,.T.);
#6148=ORIENTED_EDGE('',*,*,#4748,.F.);
#6149=ORIENTED_EDGE('',*,*,#4747,.F.);
#6150=ORIENTED_EDGE('',*,*,#4660,.T.);
#6151=ORIENTED_EDGE('',*,*,#4749,.T.);
#6152=ORIENTED_EDGE('',*,*,#4750,.T.);
#6153=ORIENTED_EDGE('',*,*,#4751,.F.);
#6154=ORIENTED_EDGE('',*,*,#4637,.T.);
#6155=ORIENTED_EDGE('',*,*,#4752,.F.);
#6156=ORIENTED_EDGE('',*,*,#4753,.F.);
#6157=ORIENTED_EDGE('',*,*,#4754,.T.);
#6158=ORIENTED_EDGE('',*,*,#4688,.T.);
#6159=ORIENTED_EDGE('',*,*,#4755,.T.);
#6160=ORIENTED_EDGE('',*,*,#4753,.T.);
#6161=ORIENTED_EDGE('',*,*,#4756,.F.);
#6162=ORIENTED_EDGE('',*,*,#4665,.T.);
#6163=ORIENTED_EDGE('',*,*,#4757,.F.);
#6164=ORIENTED_EDGE('',*,*,#4758,.F.);
#6165=ORIENTED_EDGE('',*,*,#4759,.T.);
#6166=ORIENTED_EDGE('',*,*,#4716,.T.);
#6167=ORIENTED_EDGE('',*,*,#4760,.T.);
#6168=ORIENTED_EDGE('',*,*,#4758,.T.);
#6169=ORIENTED_EDGE('',*,*,#4761,.F.);
#6170=ORIENTED_EDGE('',*,*,#4693,.T.);
#6171=ORIENTED_EDGE('',*,*,#4762,.F.);
#6172=ORIENTED_EDGE('',*,*,#4763,.F.);
#6173=ORIENTED_EDGE('',*,*,#4764,.T.);
#6174=ORIENTED_EDGE('',*,*,#4744,.T.);
#6175=ORIENTED_EDGE('',*,*,#4765,.T.);
#6176=ORIENTED_EDGE('',*,*,#4763,.T.);
#6177=ORIENTED_EDGE('',*,*,#4766,.F.);
#6178=ORIENTED_EDGE('',*,*,#4721,.T.);
#6179=ORIENTED_EDGE('',*,*,#4767,.F.);
#6180=ORIENTED_EDGE('',*,*,#4750,.F.);
#6181=ORIENTED_EDGE('',*,*,#4768,.T.);
#6182=ORIENTED_EDGE('',*,*,#4636,.T.);
#6183=ORIENTED_EDGE('',*,*,#4640,.T.);
#6184=ORIENTED_EDGE('',*,*,#4643,.T.);
#6185=ORIENTED_EDGE('',*,*,#4646,.T.);
#6186=ORIENTED_EDGE('',*,*,#4649,.T.);
#6187=ORIENTED_EDGE('',*,*,#4652,.T.);
#6188=ORIENTED_EDGE('',*,*,#4655,.T.);
#6189=ORIENTED_EDGE('',*,*,#4658,.T.);
#6190=ORIENTED_EDGE('',*,*,#4661,.T.);
#6191=ORIENTED_EDGE('',*,*,#4751,.T.);
#6192=ORIENTED_EDGE('',*,*,#4767,.T.);
#6193=ORIENTED_EDGE('',*,*,#4720,.T.);
#6194=ORIENTED_EDGE('',*,*,#4724,.T.);
#6195=ORIENTED_EDGE('',*,*,#4727,.T.);
#6196=ORIENTED_EDGE('',*,*,#4730,.T.);
#6197=ORIENTED_EDGE('',*,*,#4733,.T.);
#6198=ORIENTED_EDGE('',*,*,#4736,.T.);
#6199=ORIENTED_EDGE('',*,*,#4739,.T.);
#6200=ORIENTED_EDGE('',*,*,#4742,.T.);
#6201=ORIENTED_EDGE('',*,*,#4745,.T.);
#6202=ORIENTED_EDGE('',*,*,#4766,.T.);
#6203=ORIENTED_EDGE('',*,*,#4762,.T.);
#6204=ORIENTED_EDGE('',*,*,#4692,.T.);
#6205=ORIENTED_EDGE('',*,*,#4696,.T.);
#6206=ORIENTED_EDGE('',*,*,#4699,.T.);
#6207=ORIENTED_EDGE('',*,*,#4702,.T.);
#6208=ORIENTED_EDGE('',*,*,#4705,.T.);
#6209=ORIENTED_EDGE('',*,*,#4708,.T.);
#6210=ORIENTED_EDGE('',*,*,#4711,.T.);
#6211=ORIENTED_EDGE('',*,*,#4714,.T.);
#6212=ORIENTED_EDGE('',*,*,#4717,.T.);
#6213=ORIENTED_EDGE('',*,*,#4761,.T.);
#6214=ORIENTED_EDGE('',*,*,#4757,.T.);
#6215=ORIENTED_EDGE('',*,*,#4664,.T.);
#6216=ORIENTED_EDGE('',*,*,#4668,.T.);
#6217=ORIENTED_EDGE('',*,*,#4671,.T.);
#6218=ORIENTED_EDGE('',*,*,#4674,.T.);
#6219=ORIENTED_EDGE('',*,*,#4677,.T.);
#6220=ORIENTED_EDGE('',*,*,#4680,.T.);
#6221=ORIENTED_EDGE('',*,*,#4683,.T.);
#6222=ORIENTED_EDGE('',*,*,#4686,.T.);
#6223=ORIENTED_EDGE('',*,*,#4689,.T.);
#6224=ORIENTED_EDGE('',*,*,#4756,.T.);
#6225=ORIENTED_EDGE('',*,*,#4752,.T.);
#6226=ORIENTED_EDGE('',*,*,#4748,.T.);
#6227=ORIENTED_EDGE('',*,*,#4634,.T.);
#6228=ORIENTED_EDGE('',*,*,#4754,.F.);
#6229=ORIENTED_EDGE('',*,*,#4755,.F.);
#6230=ORIENTED_EDGE('',*,*,#4687,.T.);
#6231=ORIENTED_EDGE('',*,*,#4684,.T.);
#6232=ORIENTED_EDGE('',*,*,#4681,.T.);
#6233=ORIENTED_EDGE('',*,*,#4678,.T.);
#6234=ORIENTED_EDGE('',*,*,#4675,.T.);
#6235=ORIENTED_EDGE('',*,*,#4672,.T.);
#6236=ORIENTED_EDGE('',*,*,#4669,.T.);
#6237=ORIENTED_EDGE('',*,*,#4666,.T.);
#6238=ORIENTED_EDGE('',*,*,#4662,.T.);
#6239=ORIENTED_EDGE('',*,*,#4759,.F.);
#6240=ORIENTED_EDGE('',*,*,#4760,.F.);
#6241=ORIENTED_EDGE('',*,*,#4715,.T.);
#6242=ORIENTED_EDGE('',*,*,#4712,.T.);
#6243=ORIENTED_EDGE('',*,*,#4709,.T.);
#6244=ORIENTED_EDGE('',*,*,#4706,.T.);
#6245=ORIENTED_EDGE('',*,*,#4703,.T.);
#6246=ORIENTED_EDGE('',*,*,#4700,.T.);
#6247=ORIENTED_EDGE('',*,*,#4697,.T.);
#6248=ORIENTED_EDGE('',*,*,#4694,.T.);
#6249=ORIENTED_EDGE('',*,*,#4690,.T.);
#6250=ORIENTED_EDGE('',*,*,#4764,.F.);
#6251=ORIENTED_EDGE('',*,*,#4765,.F.);
#6252=ORIENTED_EDGE('',*,*,#4743,.T.);
#6253=ORIENTED_EDGE('',*,*,#4740,.T.);
#6254=ORIENTED_EDGE('',*,*,#4737,.T.);
#6255=ORIENTED_EDGE('',*,*,#4734,.T.);
#6256=ORIENTED_EDGE('',*,*,#4731,.T.);
#6257=ORIENTED_EDGE('',*,*,#4728,.T.);
#6258=ORIENTED_EDGE('',*,*,#4725,.T.);
#6259=ORIENTED_EDGE('',*,*,#4722,.T.);
#6260=ORIENTED_EDGE('',*,*,#4718,.T.);
#6261=ORIENTED_EDGE('',*,*,#4768,.F.);
#6262=ORIENTED_EDGE('',*,*,#4749,.F.);
#6263=ORIENTED_EDGE('',*,*,#4659,.T.);
#6264=ORIENTED_EDGE('',*,*,#4656,.T.);
#6265=ORIENTED_EDGE('',*,*,#4653,.T.);
#6266=ORIENTED_EDGE('',*,*,#4650,.T.);
#6267=ORIENTED_EDGE('',*,*,#4647,.T.);
#6268=ORIENTED_EDGE('',*,*,#4644,.T.);
#6269=ORIENTED_EDGE('',*,*,#4641,.T.);
#6270=ORIENTED_EDGE('',*,*,#4638,.T.);
#6271=ORIENTED_EDGE('',*,*,#4746,.T.);
#6272=ORIENTED_EDGE('',*,*,#4769,.F.);
#6273=ORIENTED_EDGE('',*,*,#4770,.F.);
#6274=ORIENTED_EDGE('',*,*,#4771,.T.);
#6275=ORIENTED_EDGE('',*,*,#4769,.T.);
#6276=ORIENTED_EDGE('',*,*,#4771,.F.);
#6277=ORIENTED_EDGE('',*,*,#4772,.F.);
#6278=ORIENTED_EDGE('',*,*,#4773,.T.);
#6279=ORIENTED_EDGE('',*,*,#4770,.T.);
#6280=ORIENTED_EDGE('',*,*,#4773,.F.);
#6281=ORIENTED_EDGE('',*,*,#4774,.F.);
#6282=ORIENTED_EDGE('',*,*,#4775,.T.);
#6283=ORIENTED_EDGE('',*,*,#4772,.T.);
#6284=ORIENTED_EDGE('',*,*,#4775,.F.);
#6285=ORIENTED_EDGE('',*,*,#4774,.T.);
#6286=ORIENTED_EDGE('',*,*,#4776,.F.);
#6287=ORIENTED_EDGE('',*,*,#4777,.F.);
#6288=ORIENTED_EDGE('',*,*,#4778,.T.);
#6289=ORIENTED_EDGE('',*,*,#4776,.T.);
#6290=ORIENTED_EDGE('',*,*,#4778,.F.);
#6291=ORIENTED_EDGE('',*,*,#4779,.F.);
#6292=ORIENTED_EDGE('',*,*,#4780,.T.);
#6293=ORIENTED_EDGE('',*,*,#4777,.T.);
#6294=ORIENTED_EDGE('',*,*,#4780,.F.);
#6295=ORIENTED_EDGE('',*,*,#4781,.F.);
#6296=ORIENTED_EDGE('',*,*,#4782,.T.);
#6297=ORIENTED_EDGE('',*,*,#4779,.T.);
#6298=ORIENTED_EDGE('',*,*,#4782,.F.);
#6299=ORIENTED_EDGE('',*,*,#4781,.T.);
#6300=ORIENTED_EDGE('',*,*,#4783,.T.);
#6301=ORIENTED_EDGE('',*,*,#4784,.T.);
#6302=ORIENTED_EDGE('',*,*,#4785,.T.);
#6303=ORIENTED_EDGE('',*,*,#4786,.F.);
#6304=ORIENTED_EDGE('',*,*,#4787,.T.);
#6305=ORIENTED_EDGE('',*,*,#4788,.T.);
#6306=ORIENTED_EDGE('',*,*,#4789,.T.);
#6307=ORIENTED_EDGE('',*,*,#4784,.F.);
#6308=ORIENTED_EDGE('',*,*,#4790,.T.);
#6309=ORIENTED_EDGE('',*,*,#4791,.T.);
#6310=ORIENTED_EDGE('',*,*,#4792,.T.);
#6311=ORIENTED_EDGE('',*,*,#4788,.F.);
#6312=ORIENTED_EDGE('',*,*,#4793,.T.);
#6313=ORIENTED_EDGE('',*,*,#4794,.T.);
#6314=ORIENTED_EDGE('',*,*,#4795,.T.);
#6315=ORIENTED_EDGE('',*,*,#4791,.F.);
#6316=ORIENTED_EDGE('',*,*,#4796,.T.);
#6317=ORIENTED_EDGE('',*,*,#4797,.T.);
#6318=ORIENTED_EDGE('',*,*,#4798,.T.);
#6319=ORIENTED_EDGE('',*,*,#4794,.F.);
#6320=ORIENTED_EDGE('',*,*,#4799,.T.);
#6321=ORIENTED_EDGE('',*,*,#4786,.T.);
#6322=ORIENTED_EDGE('',*,*,#4800,.T.);
#6323=ORIENTED_EDGE('',*,*,#4797,.F.);
#6324=ORIENTED_EDGE('',*,*,#4799,.F.);
#6325=ORIENTED_EDGE('',*,*,#4796,.F.);
#6326=ORIENTED_EDGE('',*,*,#4793,.F.);
#6327=ORIENTED_EDGE('',*,*,#4790,.F.);
#6328=ORIENTED_EDGE('',*,*,#4787,.F.);
#6329=ORIENTED_EDGE('',*,*,#4783,.F.);
#6330=ORIENTED_EDGE('',*,*,#4800,.F.);
#6331=ORIENTED_EDGE('',*,*,#4785,.F.);
#6332=ORIENTED_EDGE('',*,*,#4789,.F.);
#6333=ORIENTED_EDGE('',*,*,#4792,.F.);
#6334=ORIENTED_EDGE('',*,*,#4795,.F.);
#6335=ORIENTED_EDGE('',*,*,#4798,.F.);
#6336=ORIENTED_EDGE('',*,*,#4801,.F.);
#6337=ORIENTED_EDGE('',*,*,#4802,.T.);
#6338=ORIENTED_EDGE('',*,*,#4803,.F.);
#6339=ORIENTED_EDGE('',*,*,#4802,.F.);
#6340=ORIENTED_EDGE('',*,*,#4801,.T.);
#6341=ORIENTED_EDGE('',*,*,#4804,.F.);
#6342=ORIENTED_EDGE('',*,*,#4805,.F.);
#6343=ORIENTED_EDGE('',*,*,#4806,.T.);
#6344=ORIENTED_EDGE('',*,*,#4807,.F.);
#6345=ORIENTED_EDGE('',*,*,#4806,.F.);
#6346=ORIENTED_EDGE('',*,*,#4805,.T.);
#6347=ORIENTED_EDGE('',*,*,#4808,.F.);
#6348=ORIENTED_EDGE('',*,*,#4809,.F.);
#6349=ORIENTED_EDGE('',*,*,#4810,.T.);
#6350=ORIENTED_EDGE('',*,*,#4811,.F.);
#6351=ORIENTED_EDGE('',*,*,#4810,.F.);
#6352=ORIENTED_EDGE('',*,*,#4809,.T.);
#6353=ORIENTED_EDGE('',*,*,#4812,.F.);
#6354=ORIENTED_EDGE('',*,*,#4813,.F.);
#6355=ORIENTED_EDGE('',*,*,#4814,.T.);
#6356=ORIENTED_EDGE('',*,*,#4815,.F.);
#6357=ORIENTED_EDGE('',*,*,#4814,.F.);
#6358=ORIENTED_EDGE('',*,*,#4813,.T.);
#6359=ORIENTED_EDGE('',*,*,#4816,.F.);
#6360=ORIENTED_EDGE('',*,*,#4817,.F.);
#6361=ORIENTED_EDGE('',*,*,#4818,.T.);
#6362=ORIENTED_EDGE('',*,*,#4804,.T.);
#6363=ORIENTED_EDGE('',*,*,#4818,.F.);
#6364=ORIENTED_EDGE('',*,*,#4819,.F.);
#6365=ORIENTED_EDGE('',*,*,#4820,.T.);
#6366=ORIENTED_EDGE('',*,*,#4808,.T.);
#6367=ORIENTED_EDGE('',*,*,#4820,.F.);
#6368=ORIENTED_EDGE('',*,*,#4821,.F.);
#6369=ORIENTED_EDGE('',*,*,#4822,.T.);
#6370=ORIENTED_EDGE('',*,*,#4812,.T.);
#6371=ORIENTED_EDGE('',*,*,#4822,.F.);
#6372=ORIENTED_EDGE('',*,*,#4823,.F.);
#6373=ORIENTED_EDGE('',*,*,#4824,.T.);
#6374=ORIENTED_EDGE('',*,*,#4816,.T.);
#6375=ORIENTED_EDGE('',*,*,#4824,.F.);
#6376=ORIENTED_EDGE('',*,*,#4825,.T.);
#6377=ORIENTED_EDGE('',*,*,#4826,.T.);
#6378=ORIENTED_EDGE('',*,*,#4827,.F.);
#6379=ORIENTED_EDGE('',*,*,#4828,.F.);
#6380=ORIENTED_EDGE('',*,*,#4829,.T.);
#6381=ORIENTED_EDGE('',*,*,#4828,.T.);
#6382=ORIENTED_EDGE('',*,*,#4830,.F.);
#6383=ORIENTED_EDGE('',*,*,#4831,.F.);
#6384=ORIENTED_EDGE('',*,*,#4832,.T.);
#6385=ORIENTED_EDGE('',*,*,#4831,.T.);
#6386=ORIENTED_EDGE('',*,*,#4833,.F.);
#6387=ORIENTED_EDGE('',*,*,#4834,.F.);
#6388=ORIENTED_EDGE('',*,*,#4835,.T.);
#6389=ORIENTED_EDGE('',*,*,#4834,.T.);
#6390=ORIENTED_EDGE('',*,*,#4836,.F.);
#6391=ORIENTED_EDGE('',*,*,#4837,.F.);
#6392=ORIENTED_EDGE('',*,*,#4838,.T.);
#6393=ORIENTED_EDGE('',*,*,#4837,.T.);
#6394=ORIENTED_EDGE('',*,*,#4839,.F.);
#6395=ORIENTED_EDGE('',*,*,#4840,.F.);
#6396=ORIENTED_EDGE('',*,*,#4815,.T.);
#6397=ORIENTED_EDGE('',*,*,#4811,.T.);
#6398=ORIENTED_EDGE('',*,*,#4807,.T.);
#6399=ORIENTED_EDGE('',*,*,#4803,.T.);
#6400=ORIENTED_EDGE('',*,*,#4841,.T.);
#6401=ORIENTED_EDGE('',*,*,#4840,.T.);
#6402=ORIENTED_EDGE('',*,*,#4842,.F.);
#6403=ORIENTED_EDGE('',*,*,#4843,.F.);
#6404=ORIENTED_EDGE('',*,*,#4844,.T.);
#6405=ORIENTED_EDGE('',*,*,#4843,.T.);
#6406=ORIENTED_EDGE('',*,*,#4845,.F.);
#6407=ORIENTED_EDGE('',*,*,#4846,.F.);
#6408=ORIENTED_EDGE('',*,*,#4847,.T.);
#6409=ORIENTED_EDGE('',*,*,#4846,.T.);
#6410=ORIENTED_EDGE('',*,*,#4848,.F.);
#6411=ORIENTED_EDGE('',*,*,#4849,.F.);
#6412=ORIENTED_EDGE('',*,*,#4850,.T.);
#6413=ORIENTED_EDGE('',*,*,#4849,.T.);
#6414=ORIENTED_EDGE('',*,*,#4851,.F.);
#6415=ORIENTED_EDGE('',*,*,#4852,.F.);
#6416=ORIENTED_EDGE('',*,*,#4853,.T.);
#6417=ORIENTED_EDGE('',*,*,#4852,.T.);
#6418=ORIENTED_EDGE('',*,*,#4854,.F.);
#6419=ORIENTED_EDGE('',*,*,#4855,.F.);
#6420=ORIENTED_EDGE('',*,*,#4856,.T.);
#6421=ORIENTED_EDGE('',*,*,#4855,.T.);
#6422=ORIENTED_EDGE('',*,*,#4857,.F.);
#6423=ORIENTED_EDGE('',*,*,#4858,.F.);
#6424=ORIENTED_EDGE('',*,*,#4817,.T.);
#6425=ORIENTED_EDGE('',*,*,#4819,.T.);
#6426=ORIENTED_EDGE('',*,*,#4821,.T.);
#6427=ORIENTED_EDGE('',*,*,#4823,.T.);
#6428=ORIENTED_EDGE('',*,*,#4859,.T.);
#6429=ORIENTED_EDGE('',*,*,#4858,.T.);
#6430=ORIENTED_EDGE('',*,*,#4860,.F.);
#6431=ORIENTED_EDGE('',*,*,#4826,.F.);
#6432=ORIENTED_EDGE('',*,*,#4860,.T.);
#6433=ORIENTED_EDGE('',*,*,#4857,.T.);
#6434=ORIENTED_EDGE('',*,*,#4854,.T.);
#6435=ORIENTED_EDGE('',*,*,#4851,.T.);
#6436=ORIENTED_EDGE('',*,*,#4848,.T.);
#6437=ORIENTED_EDGE('',*,*,#4845,.T.);
#6438=ORIENTED_EDGE('',*,*,#4842,.T.);
#6439=ORIENTED_EDGE('',*,*,#4839,.T.);
#6440=ORIENTED_EDGE('',*,*,#4836,.T.);
#6441=ORIENTED_EDGE('',*,*,#4833,.T.);
#6442=ORIENTED_EDGE('',*,*,#4830,.T.);
#6443=ORIENTED_EDGE('',*,*,#4827,.T.);
#6444=ORIENTED_EDGE('',*,*,#4859,.F.);
#6445=ORIENTED_EDGE('',*,*,#4825,.F.);
#6446=ORIENTED_EDGE('',*,*,#4829,.F.);
#6447=ORIENTED_EDGE('',*,*,#4832,.F.);
#6448=ORIENTED_EDGE('',*,*,#4835,.F.);
#6449=ORIENTED_EDGE('',*,*,#4838,.F.);
#6450=ORIENTED_EDGE('',*,*,#4841,.F.);
#6451=ORIENTED_EDGE('',*,*,#4844,.F.);
#6452=ORIENTED_EDGE('',*,*,#4847,.F.);
#6453=ORIENTED_EDGE('',*,*,#4850,.F.);
#6454=ORIENTED_EDGE('',*,*,#4853,.F.);
#6455=ORIENTED_EDGE('',*,*,#4856,.F.);
#6456=ORIENTED_EDGE('',*,*,#4861,.F.);
#6457=ORIENTED_EDGE('',*,*,#4862,.F.);
#6458=ORIENTED_EDGE('',*,*,#4863,.F.);
#6459=ORIENTED_EDGE('',*,*,#4864,.F.);
#6460=ORIENTED_EDGE('',*,*,#4863,.T.);
#6461=ORIENTED_EDGE('',*,*,#4865,.T.);
#6462=ORIENTED_EDGE('',*,*,#4866,.F.);
#6463=ORIENTED_EDGE('',*,*,#4867,.F.);
#6464=ORIENTED_EDGE('',*,*,#4868,.T.);
#6465=ORIENTED_EDGE('',*,*,#4869,.T.);
#6466=ORIENTED_EDGE('',*,*,#4870,.T.);
#6467=ORIENTED_EDGE('',*,*,#4866,.T.);
#6468=ORIENTED_EDGE('',*,*,#4871,.T.);
#6469=ORIENTED_EDGE('',*,*,#4868,.F.);
#6470=ORIENTED_EDGE('',*,*,#4865,.F.);
#6471=ORIENTED_EDGE('',*,*,#4862,.T.);
#6472=ORIENTED_EDGE('',*,*,#4872,.F.);
#6473=ORIENTED_EDGE('',*,*,#4873,.F.);
#6474=ORIENTED_EDGE('',*,*,#4874,.T.);
#6475=ORIENTED_EDGE('',*,*,#4875,.F.);
#6476=ORIENTED_EDGE('',*,*,#4876,.T.);
#6477=ORIENTED_EDGE('',*,*,#4877,.T.);
#6478=ORIENTED_EDGE('',*,*,#4878,.T.);
#6479=ORIENTED_EDGE('',*,*,#4879,.T.);
#6480=ORIENTED_EDGE('',*,*,#4880,.T.);
#6481=ORIENTED_EDGE('',*,*,#4869,.F.);
#6482=ORIENTED_EDGE('',*,*,#4878,.F.);
#6483=ORIENTED_EDGE('',*,*,#4881,.F.);
#6484=ORIENTED_EDGE('',*,*,#4882,.F.);
#6485=ORIENTED_EDGE('',*,*,#4879,.F.);
#6486=ORIENTED_EDGE('',*,*,#4877,.F.);
#6487=ORIENTED_EDGE('',*,*,#4870,.F.);
#6488=ORIENTED_EDGE('',*,*,#4880,.F.);
#6489=ORIENTED_EDGE('',*,*,#4882,.T.);
#6490=ORIENTED_EDGE('',*,*,#4883,.F.);
#6491=ORIENTED_EDGE('',*,*,#4884,.F.);
#6492=ORIENTED_EDGE('',*,*,#4885,.T.);
#6493=ORIENTED_EDGE('',*,*,#4886,.F.);
#6494=ORIENTED_EDGE('',*,*,#4887,.T.);
#6495=ORIENTED_EDGE('',*,*,#4864,.T.);
#6496=ORIENTED_EDGE('',*,*,#4867,.T.);
#6497=ORIENTED_EDGE('',*,*,#4881,.T.);
#6498=ORIENTED_EDGE('',*,*,#4876,.F.);
#6499=ORIENTED_EDGE('',*,*,#4888,.F.);
#6500=ORIENTED_EDGE('',*,*,#4883,.T.);
#6501=ORIENTED_EDGE('',*,*,#4884,.T.);
#6502=ORIENTED_EDGE('',*,*,#4888,.T.);
#6503=ORIENTED_EDGE('',*,*,#4875,.T.);
#6504=ORIENTED_EDGE('',*,*,#4889,.T.);
#6505=ORIENTED_EDGE('',*,*,#4890,.T.);
#6506=ORIENTED_EDGE('',*,*,#4891,.T.);
#6507=ORIENTED_EDGE('',*,*,#4890,.F.);
#6508=ORIENTED_EDGE('',*,*,#4892,.F.);
#6509=ORIENTED_EDGE('',*,*,#4893,.T.);
#6510=ORIENTED_EDGE('',*,*,#4871,.F.);
#6511=ORIENTED_EDGE('',*,*,#4893,.F.);
#6512=ORIENTED_EDGE('',*,*,#4894,.F.);
#6513=ORIENTED_EDGE('',*,*,#4895,.F.);
#6514=ORIENTED_EDGE('',*,*,#4896,.F.);
#6515=ORIENTED_EDGE('',*,*,#4889,.F.);
#6516=ORIENTED_EDGE('',*,*,#4874,.F.);
#6517=ORIENTED_EDGE('',*,*,#4897,.F.);
#6518=ORIENTED_EDGE('',*,*,#4894,.T.);
#6519=ORIENTED_EDGE('',*,*,#4892,.T.);
#6520=ORIENTED_EDGE('',*,*,#4891,.F.);
#6521=ORIENTED_EDGE('',*,*,#4896,.T.);
#6522=ORIENTED_EDGE('',*,*,#4898,.F.);
#6523=ORIENTED_EDGE('',*,*,#4885,.F.);
#6524=ORIENTED_EDGE('',*,*,#4873,.T.);
#6525=ORIENTED_EDGE('',*,*,#4899,.T.);
#6526=ORIENTED_EDGE('',*,*,#4886,.T.);
#6527=ORIENTED_EDGE('',*,*,#4898,.T.);
#6528=ORIENTED_EDGE('',*,*,#4895,.T.);
#6529=ORIENTED_EDGE('',*,*,#4897,.T.);
#6530=ORIENTED_EDGE('',*,*,#4861,.T.);
#6531=ORIENTED_EDGE('',*,*,#4887,.F.);
#6532=ORIENTED_EDGE('',*,*,#4899,.F.);
#6533=ORIENTED_EDGE('',*,*,#4872,.T.);
#6534=ORIENTED_EDGE('',*,*,#4900,.T.);
#6535=ORIENTED_EDGE('',*,*,#4901,.T.);
#6536=ORIENTED_EDGE('',*,*,#4902,.T.);
#6537=ORIENTED_EDGE('',*,*,#4901,.F.);
#6538=ORIENTED_EDGE('',*,*,#4902,.F.);
#6539=ORIENTED_EDGE('',*,*,#4903,.T.);
#6540=ORIENTED_EDGE('',*,*,#4904,.T.);
#6541=ORIENTED_EDGE('',*,*,#4903,.F.);
#6542=ORIENTED_EDGE('',*,*,#4905,.T.);
#6543=ORIENTED_EDGE('',*,*,#4900,.F.);
#6544=ORIENTED_EDGE('',*,*,#4905,.F.);
#6545=ORIENTED_EDGE('',*,*,#4906,.T.);
#6546=ORIENTED_EDGE('',*,*,#4907,.T.);
#6547=ORIENTED_EDGE('',*,*,#4906,.F.);
#6548=ORIENTED_EDGE('',*,*,#4907,.F.);
#6549=ORIENTED_EDGE('',*,*,#4904,.F.);
#6550=ORIENTED_EDGE('',*,*,#4908,.T.);
#6551=ORIENTED_EDGE('',*,*,#4909,.T.);
#6552=ORIENTED_EDGE('',*,*,#4910,.T.);
#6553=ORIENTED_EDGE('',*,*,#4911,.F.);
#6554=ORIENTED_EDGE('',*,*,#4912,.T.);
#6555=ORIENTED_EDGE('',*,*,#4913,.T.);
#6556=ORIENTED_EDGE('',*,*,#4914,.T.);
#6557=ORIENTED_EDGE('',*,*,#4909,.F.);
#6558=ORIENTED_EDGE('',*,*,#4915,.T.);
#6559=ORIENTED_EDGE('',*,*,#4916,.T.);
#6560=ORIENTED_EDGE('',*,*,#4917,.T.);
#6561=ORIENTED_EDGE('',*,*,#4913,.F.);
#6562=ORIENTED_EDGE('',*,*,#4918,.T.);
#6563=ORIENTED_EDGE('',*,*,#4919,.T.);
#6564=ORIENTED_EDGE('',*,*,#4920,.T.);
#6565=ORIENTED_EDGE('',*,*,#4916,.F.);
#6566=ORIENTED_EDGE('',*,*,#4921,.T.);
#6567=ORIENTED_EDGE('',*,*,#4922,.T.);
#6568=ORIENTED_EDGE('',*,*,#4923,.T.);
#6569=ORIENTED_EDGE('',*,*,#4919,.F.);
#6570=ORIENTED_EDGE('',*,*,#4924,.T.);
#6571=ORIENTED_EDGE('',*,*,#4911,.T.);
#6572=ORIENTED_EDGE('',*,*,#4925,.T.);
#6573=ORIENTED_EDGE('',*,*,#4922,.F.);
#6574=ORIENTED_EDGE('',*,*,#4924,.F.);
#6575=ORIENTED_EDGE('',*,*,#4921,.F.);
#6576=ORIENTED_EDGE('',*,*,#4918,.F.);
#6577=ORIENTED_EDGE('',*,*,#4915,.F.);
#6578=ORIENTED_EDGE('',*,*,#4912,.F.);
#6579=ORIENTED_EDGE('',*,*,#4908,.F.);
#6580=ORIENTED_EDGE('',*,*,#4925,.F.);
#6581=ORIENTED_EDGE('',*,*,#4910,.F.);
#6582=ORIENTED_EDGE('',*,*,#4914,.F.);
#6583=ORIENTED_EDGE('',*,*,#4917,.F.);
#6584=ORIENTED_EDGE('',*,*,#4920,.F.);
#6585=ORIENTED_EDGE('',*,*,#4923,.F.);
#6586=ORIENTED_EDGE('',*,*,#4926,.T.);
#6587=ORIENTED_EDGE('',*,*,#4927,.F.);
#6588=ORIENTED_EDGE('',*,*,#4926,.F.);
#6589=ORIENTED_EDGE('',*,*,#4928,.T.);
#6590=ORIENTED_EDGE('',*,*,#4929,.T.);
#6591=ORIENTED_EDGE('',*,*,#4928,.F.);
#6592=ORIENTED_EDGE('',*,*,#4929,.F.);
#6593=ORIENTED_EDGE('',*,*,#4930,.F.);
#6594=ORIENTED_EDGE('',*,*,#4931,.F.);
#6595=ORIENTED_EDGE('',*,*,#4932,.T.);
#6596=ORIENTED_EDGE('',*,*,#4930,.T.);
#6597=ORIENTED_EDGE('',*,*,#4932,.F.);
#6598=ORIENTED_EDGE('',*,*,#4933,.F.);
#6599=ORIENTED_EDGE('',*,*,#4934,.T.);
#6600=ORIENTED_EDGE('',*,*,#4931,.T.);
#6601=ORIENTED_EDGE('',*,*,#4934,.F.);
#6602=ORIENTED_EDGE('',*,*,#4935,.F.);
#6603=ORIENTED_EDGE('',*,*,#4936,.T.);
#6604=ORIENTED_EDGE('',*,*,#4933,.T.);
#6605=ORIENTED_EDGE('',*,*,#4936,.F.);
#6606=ORIENTED_EDGE('',*,*,#4935,.T.);
#6607=ORIENTED_EDGE('',*,*,#4937,.F.);
#6608=ORIENTED_EDGE('',*,*,#4938,.F.);
#6609=ORIENTED_EDGE('',*,*,#4939,.T.);
#6610=ORIENTED_EDGE('',*,*,#4937,.T.);
#6611=ORIENTED_EDGE('',*,*,#4939,.F.);
#6612=ORIENTED_EDGE('',*,*,#4927,.T.);
#6613=ORIENTED_EDGE('',*,*,#4940,.T.);
#6614=ORIENTED_EDGE('',*,*,#4938,.T.);
#6615=ORIENTED_EDGE('',*,*,#4940,.F.);
#6616=ORIENTED_EDGE('',*,*,#4941,.F.);
#6617=ORIENTED_EDGE('',*,*,#4942,.T.);
#6618=ORIENTED_EDGE('',*,*,#4943,.F.);
#6619=ORIENTED_EDGE('',*,*,#4942,.F.);
#6620=ORIENTED_EDGE('',*,*,#4944,.F.);
#6621=ORIENTED_EDGE('',*,*,#4945,.T.);
#6622=ORIENTED_EDGE('',*,*,#4946,.F.);
#6623=ORIENTED_EDGE('',*,*,#4945,.F.);
#6624=ORIENTED_EDGE('',*,*,#4947,.F.);
#6625=ORIENTED_EDGE('',*,*,#4948,.T.);
#6626=ORIENTED_EDGE('',*,*,#4949,.F.);
#6627=ORIENTED_EDGE('',*,*,#4948,.F.);
#6628=ORIENTED_EDGE('',*,*,#4950,.F.);
#6629=ORIENTED_EDGE('',*,*,#4951,.T.);
#6630=ORIENTED_EDGE('',*,*,#4952,.F.);
#6631=ORIENTED_EDGE('',*,*,#4951,.F.);
#6632=ORIENTED_EDGE('',*,*,#4953,.F.);
#6633=ORIENTED_EDGE('',*,*,#4954,.T.);
#6634=ORIENTED_EDGE('',*,*,#4955,.F.);
#6635=ORIENTED_EDGE('',*,*,#4954,.F.);
#6636=ORIENTED_EDGE('',*,*,#4956,.F.);
#6637=ORIENTED_EDGE('',*,*,#4957,.T.);
#6638=ORIENTED_EDGE('',*,*,#4958,.F.);
#6639=ORIENTED_EDGE('',*,*,#4957,.F.);
#6640=ORIENTED_EDGE('',*,*,#4959,.F.);
#6641=ORIENTED_EDGE('',*,*,#4960,.F.);
#6642=ORIENTED_EDGE('',*,*,#4961,.F.);
#6643=ORIENTED_EDGE('',*,*,#4962,.T.);
#6644=ORIENTED_EDGE('',*,*,#4963,.F.);
#6645=ORIENTED_EDGE('',*,*,#4964,.T.);
#6646=ORIENTED_EDGE('',*,*,#4965,.T.);
#6647=ORIENTED_EDGE('',*,*,#4966,.F.);
#6648=ORIENTED_EDGE('',*,*,#4967,.T.);
#6649=ORIENTED_EDGE('',*,*,#4961,.T.);
#6650=ORIENTED_EDGE('',*,*,#4968,.F.);
#6651=ORIENTED_EDGE('',*,*,#4965,.F.);
#6652=ORIENTED_EDGE('',*,*,#4969,.F.);
#6653=ORIENTED_EDGE('',*,*,#4970,.F.);
#6654=ORIENTED_EDGE('',*,*,#4971,.F.);
#6655=ORIENTED_EDGE('',*,*,#4972,.F.);
#6656=ORIENTED_EDGE('',*,*,#4973,.F.);
#6657=ORIENTED_EDGE('',*,*,#4962,.F.);
#6658=ORIENTED_EDGE('',*,*,#4967,.F.);
#6659=ORIENTED_EDGE('',*,*,#4964,.F.);
#6660=ORIENTED_EDGE('',*,*,#4941,.T.);
#6661=ORIENTED_EDGE('',*,*,#4944,.T.);
#6662=ORIENTED_EDGE('',*,*,#4947,.T.);
#6663=ORIENTED_EDGE('',*,*,#4950,.T.);
#6664=ORIENTED_EDGE('',*,*,#4953,.T.);
#6665=ORIENTED_EDGE('',*,*,#4956,.T.);
#6666=ORIENTED_EDGE('',*,*,#4963,.T.);
#6667=ORIENTED_EDGE('',*,*,#4974,.F.);
#6668=ORIENTED_EDGE('',*,*,#4975,.F.);
#6669=ORIENTED_EDGE('',*,*,#4969,.T.);
#6670=ORIENTED_EDGE('',*,*,#4972,.T.);
#6671=ORIENTED_EDGE('',*,*,#4976,.T.);
#6672=ORIENTED_EDGE('',*,*,#4977,.F.);
#6673=ORIENTED_EDGE('',*,*,#4978,.F.);
#6674=ORIENTED_EDGE('',*,*,#4959,.T.);
#6675=ORIENTED_EDGE('',*,*,#4973,.T.);
#6676=ORIENTED_EDGE('',*,*,#4978,.T.);
#6677=ORIENTED_EDGE('',*,*,#4979,.F.);
#6678=ORIENTED_EDGE('',*,*,#4970,.T.);
#6679=ORIENTED_EDGE('',*,*,#4975,.T.);
#6680=ORIENTED_EDGE('',*,*,#4980,.F.);
#6681=ORIENTED_EDGE('',*,*,#4981,.F.);
#6682=ORIENTED_EDGE('',*,*,#4971,.T.);
#6683=ORIENTED_EDGE('',*,*,#4981,.T.);
#6684=ORIENTED_EDGE('',*,*,#4982,.F.);
#6685=ORIENTED_EDGE('',*,*,#4976,.F.);
#6686=ORIENTED_EDGE('',*,*,#4979,.T.);
#6687=ORIENTED_EDGE('',*,*,#4977,.T.);
#6688=ORIENTED_EDGE('',*,*,#4982,.T.);
#6689=ORIENTED_EDGE('',*,*,#4980,.T.);
#6690=ORIENTED_EDGE('',*,*,#4974,.T.);
#6691=ORIENTED_EDGE('',*,*,#4966,.T.);
#6692=ORIENTED_EDGE('',*,*,#4968,.T.);
#6693=ORIENTED_EDGE('',*,*,#4960,.T.);
#6694=ORIENTED_EDGE('',*,*,#4943,.T.);
#6695=ORIENTED_EDGE('',*,*,#4946,.T.);
#6696=ORIENTED_EDGE('',*,*,#4949,.T.);
#6697=ORIENTED_EDGE('',*,*,#4952,.T.);
#6698=ORIENTED_EDGE('',*,*,#4955,.T.);
#6699=ORIENTED_EDGE('',*,*,#4958,.T.);
#6700=ORIENTED_EDGE('',*,*,#4983,.F.);
#6701=ORIENTED_EDGE('',*,*,#4984,.T.);
#6702=ORIENTED_EDGE('',*,*,#4985,.F.);
#6703=ORIENTED_EDGE('',*,*,#4984,.F.);
#6704=ORIENTED_EDGE('',*,*,#4983,.T.);
#6705=ORIENTED_EDGE('',*,*,#4986,.F.);
#6706=ORIENTED_EDGE('',*,*,#4987,.T.);
#6707=ORIENTED_EDGE('',*,*,#4988,.F.);
#6708=ORIENTED_EDGE('',*,*,#4987,.F.);
#6709=ORIENTED_EDGE('',*,*,#4986,.T.);
#6710=ORIENTED_EDGE('',*,*,#4989,.F.);
#6711=ORIENTED_EDGE('',*,*,#4990,.T.);
#6712=ORIENTED_EDGE('',*,*,#4991,.F.);
#6713=ORIENTED_EDGE('',*,*,#4992,.T.);
#6714=ORIENTED_EDGE('',*,*,#4990,.F.);
#6715=ORIENTED_EDGE('',*,*,#4989,.T.);
#6716=ORIENTED_EDGE('',*,*,#4988,.T.);
#6717=ORIENTED_EDGE('',*,*,#4993,.F.);
#6718=ORIENTED_EDGE('',*,*,#4992,.F.);
#6719=ORIENTED_EDGE('',*,*,#4993,.T.);
#6720=ORIENTED_EDGE('',*,*,#4994,.T.);
#6721=ORIENTED_EDGE('',*,*,#4995,.T.);
#6722=ORIENTED_EDGE('',*,*,#4996,.F.);
#6723=ORIENTED_EDGE('',*,*,#4997,.T.);
#6724=ORIENTED_EDGE('',*,*,#4998,.T.);
#6725=ORIENTED_EDGE('',*,*,#4999,.F.);
#6726=ORIENTED_EDGE('',*,*,#4997,.F.);
#6727=ORIENTED_EDGE('',*,*,#4996,.T.);
#6728=ORIENTED_EDGE('',*,*,#4985,.T.);
#6729=ORIENTED_EDGE('',*,*,#5000,.F.);
#6730=ORIENTED_EDGE('',*,*,#4998,.F.);
#6731=ORIENTED_EDGE('',*,*,#5000,.T.);
#6732=ORIENTED_EDGE('',*,*,#5001,.F.);
#6733=ORIENTED_EDGE('',*,*,#5002,.F.);
#6734=ORIENTED_EDGE('',*,*,#4991,.T.);
#6735=ORIENTED_EDGE('',*,*,#4995,.F.);
#6736=ORIENTED_EDGE('',*,*,#5003,.T.);
#6737=ORIENTED_EDGE('',*,*,#5001,.T.);
#6738=ORIENTED_EDGE('',*,*,#4999,.T.);
#6739=ORIENTED_EDGE('',*,*,#5002,.T.);
#6740=ORIENTED_EDGE('',*,*,#5003,.F.);
#6741=ORIENTED_EDGE('',*,*,#4994,.F.);
#6742=ORIENTED_EDGE('',*,*,#5004,.F.);
#6743=ORIENTED_EDGE('',*,*,#5005,.T.);
#6744=ORIENTED_EDGE('',*,*,#5006,.F.);
#6745=ORIENTED_EDGE('',*,*,#5007,.F.);
#6746=ORIENTED_EDGE('',*,*,#5008,.T.);
#6747=ORIENTED_EDGE('',*,*,#5009,.F.);
#6748=ORIENTED_EDGE('',*,*,#5008,.F.);
#6749=ORIENTED_EDGE('',*,*,#5010,.F.);
#6750=ORIENTED_EDGE('',*,*,#5011,.F.);
#6751=ORIENTED_EDGE('',*,*,#5005,.F.);
#6752=ORIENTED_EDGE('',*,*,#5012,.F.);
#6753=ORIENTED_EDGE('',*,*,#5013,.T.);
#6754=ORIENTED_EDGE('',*,*,#5014,.F.);
#6755=ORIENTED_EDGE('',*,*,#5015,.F.);
#6756=ORIENTED_EDGE('',*,*,#5016,.T.);
#6757=ORIENTED_EDGE('',*,*,#5017,.F.);
#6758=ORIENTED_EDGE('',*,*,#5016,.F.);
#6759=ORIENTED_EDGE('',*,*,#5018,.F.);
#6760=ORIENTED_EDGE('',*,*,#5019,.F.);
#6761=ORIENTED_EDGE('',*,*,#5013,.F.);
#6762=ORIENTED_EDGE('',*,*,#5020,.F.);
#6763=ORIENTED_EDGE('',*,*,#5021,.T.);
#6764=ORIENTED_EDGE('',*,*,#5022,.F.);
#6765=ORIENTED_EDGE('',*,*,#5023,.F.);
#6766=ORIENTED_EDGE('',*,*,#5024,.T.);
#6767=ORIENTED_EDGE('',*,*,#5025,.F.);
#6768=ORIENTED_EDGE('',*,*,#5024,.F.);
#6769=ORIENTED_EDGE('',*,*,#5026,.F.);
#6770=ORIENTED_EDGE('',*,*,#5027,.F.);
#6771=ORIENTED_EDGE('',*,*,#5021,.F.);
#6772=ORIENTED_EDGE('',*,*,#5028,.F.);
#6773=ORIENTED_EDGE('',*,*,#5029,.T.);
#6774=ORIENTED_EDGE('',*,*,#5030,.F.);
#6775=ORIENTED_EDGE('',*,*,#5031,.F.);
#6776=ORIENTED_EDGE('',*,*,#5032,.T.);
#6777=ORIENTED_EDGE('',*,*,#5033,.F.);
#6778=ORIENTED_EDGE('',*,*,#5032,.F.);
#6779=ORIENTED_EDGE('',*,*,#5034,.F.);
#6780=ORIENTED_EDGE('',*,*,#5035,.F.);
#6781=ORIENTED_EDGE('',*,*,#5029,.F.);
#6782=ORIENTED_EDGE('',*,*,#5006,.T.);
#6783=ORIENTED_EDGE('',*,*,#5004,.T.);
#6784=ORIENTED_EDGE('',*,*,#5011,.T.);
#6785=ORIENTED_EDGE('',*,*,#5036,.T.);
#6786=ORIENTED_EDGE('',*,*,#5022,.T.);
#6787=ORIENTED_EDGE('',*,*,#5020,.T.);
#6788=ORIENTED_EDGE('',*,*,#5027,.T.);
#6789=ORIENTED_EDGE('',*,*,#5037,.T.);
#6790=ORIENTED_EDGE('',*,*,#5038,.F.);
#6791=ORIENTED_EDGE('',*,*,#5039,.T.);
#6792=ORIENTED_EDGE('',*,*,#5040,.F.);
#6793=ORIENTED_EDGE('',*,*,#5041,.T.);
#6794=ORIENTED_EDGE('',*,*,#5014,.T.);
#6795=ORIENTED_EDGE('',*,*,#5012,.T.);
#6796=ORIENTED_EDGE('',*,*,#5019,.T.);
#6797=ORIENTED_EDGE('',*,*,#5042,.T.);
#6798=ORIENTED_EDGE('',*,*,#5030,.T.);
#6799=ORIENTED_EDGE('',*,*,#5028,.T.);
#6800=ORIENTED_EDGE('',*,*,#5035,.T.);
#6801=ORIENTED_EDGE('',*,*,#5043,.T.);
#6802=ORIENTED_EDGE('',*,*,#5044,.F.);
#6803=ORIENTED_EDGE('',*,*,#5045,.F.);
#6804=ORIENTED_EDGE('',*,*,#5046,.F.);
#6805=ORIENTED_EDGE('',*,*,#5047,.T.);
#6806=ORIENTED_EDGE('',*,*,#5038,.T.);
#6807=ORIENTED_EDGE('',*,*,#5048,.T.);
#6808=ORIENTED_EDGE('',*,*,#5049,.T.);
#6809=ORIENTED_EDGE('',*,*,#5050,.T.);
#6810=ORIENTED_EDGE('',*,*,#5051,.T.);
#6811=ORIENTED_EDGE('',*,*,#5052,.T.);
#6812=ORIENTED_EDGE('',*,*,#5046,.T.);
#6813=ORIENTED_EDGE('',*,*,#5053,.T.);
#6814=ORIENTED_EDGE('',*,*,#5054,.T.);
#6815=ORIENTED_EDGE('',*,*,#5055,.T.);
#6816=ORIENTED_EDGE('',*,*,#5056,.T.);
#6817=ORIENTED_EDGE('',*,*,#5057,.T.);
#6818=ORIENTED_EDGE('',*,*,#5010,.T.);
#6819=ORIENTED_EDGE('',*,*,#5007,.T.);
#6820=ORIENTED_EDGE('',*,*,#5041,.F.);
#6821=ORIENTED_EDGE('',*,*,#5058,.F.);
#6822=ORIENTED_EDGE('',*,*,#5059,.F.);
#6823=ORIENTED_EDGE('',*,*,#5048,.F.);
#6824=ORIENTED_EDGE('',*,*,#5037,.F.);
#6825=ORIENTED_EDGE('',*,*,#5026,.T.);
#6826=ORIENTED_EDGE('',*,*,#5023,.T.);
#6827=ORIENTED_EDGE('',*,*,#5036,.F.);
#6828=ORIENTED_EDGE('',*,*,#5059,.T.);
#6829=ORIENTED_EDGE('',*,*,#5060,.F.);
#6830=ORIENTED_EDGE('',*,*,#5061,.F.);
#6831=ORIENTED_EDGE('',*,*,#5049,.F.);
#6832=ORIENTED_EDGE('',*,*,#5061,.T.);
#6833=ORIENTED_EDGE('',*,*,#5062,.F.);
#6834=ORIENTED_EDGE('',*,*,#5063,.F.);
#6835=ORIENTED_EDGE('',*,*,#5050,.F.);
#6836=ORIENTED_EDGE('',*,*,#5009,.T.);
#6837=ORIENTED_EDGE('',*,*,#5017,.T.);
#6838=ORIENTED_EDGE('',*,*,#5025,.T.);
#6839=ORIENTED_EDGE('',*,*,#5033,.T.);
#6840=ORIENTED_EDGE('',*,*,#5063,.T.);
#6841=ORIENTED_EDGE('',*,*,#5064,.F.);
#6842=ORIENTED_EDGE('',*,*,#5065,.F.);
#6843=ORIENTED_EDGE('',*,*,#5051,.F.);
#6844=ORIENTED_EDGE('',*,*,#5018,.T.);
#6845=ORIENTED_EDGE('',*,*,#5015,.T.);
#6846=ORIENTED_EDGE('',*,*,#5047,.F.);
#6847=ORIENTED_EDGE('',*,*,#5052,.F.);
#6848=ORIENTED_EDGE('',*,*,#5065,.T.);
#6849=ORIENTED_EDGE('',*,*,#5066,.F.);
#6850=ORIENTED_EDGE('',*,*,#5043,.F.);
#6851=ORIENTED_EDGE('',*,*,#5034,.T.);
#6852=ORIENTED_EDGE('',*,*,#5031,.T.);
#6853=ORIENTED_EDGE('',*,*,#5042,.F.);
#6854=ORIENTED_EDGE('',*,*,#5045,.T.);
#6855=ORIENTED_EDGE('',*,*,#5067,.F.);
#6856=ORIENTED_EDGE('',*,*,#5068,.F.);
#6857=ORIENTED_EDGE('',*,*,#5053,.F.);
#6858=ORIENTED_EDGE('',*,*,#5068,.T.);
#6859=ORIENTED_EDGE('',*,*,#5069,.F.);
#6860=ORIENTED_EDGE('',*,*,#5070,.F.);
#6861=ORIENTED_EDGE('',*,*,#5054,.F.);
#6862=ORIENTED_EDGE('',*,*,#5070,.T.);
#6863=ORIENTED_EDGE('',*,*,#5071,.F.);
#6864=ORIENTED_EDGE('',*,*,#5072,.F.);
#6865=ORIENTED_EDGE('',*,*,#5055,.F.);
#6866=ORIENTED_EDGE('',*,*,#5072,.T.);
#6867=ORIENTED_EDGE('',*,*,#5073,.F.);
#6868=ORIENTED_EDGE('',*,*,#5074,.F.);
#6869=ORIENTED_EDGE('',*,*,#5056,.F.);
#6870=ORIENTED_EDGE('',*,*,#5074,.T.);
#6871=ORIENTED_EDGE('',*,*,#5075,.F.);
#6872=ORIENTED_EDGE('',*,*,#5039,.F.);
#6873=ORIENTED_EDGE('',*,*,#5057,.F.);
#6874=ORIENTED_EDGE('',*,*,#5040,.T.);
#6875=ORIENTED_EDGE('',*,*,#5075,.T.);
#6876=ORIENTED_EDGE('',*,*,#5073,.T.);
#6877=ORIENTED_EDGE('',*,*,#5071,.T.);
#6878=ORIENTED_EDGE('',*,*,#5069,.T.);
#6879=ORIENTED_EDGE('',*,*,#5067,.T.);
#6880=ORIENTED_EDGE('',*,*,#5044,.T.);
#6881=ORIENTED_EDGE('',*,*,#5066,.T.);
#6882=ORIENTED_EDGE('',*,*,#5064,.T.);
#6883=ORIENTED_EDGE('',*,*,#5062,.T.);
#6884=ORIENTED_EDGE('',*,*,#5060,.T.);
#6885=ORIENTED_EDGE('',*,*,#5058,.T.);
#6886=ORIENTED_EDGE('',*,*,#5076,.T.);
#6887=ORIENTED_EDGE('',*,*,#5077,.T.);
#6888=ORIENTED_EDGE('',*,*,#5078,.F.);
#6889=ORIENTED_EDGE('',*,*,#5079,.F.);
#6890=ORIENTED_EDGE('',*,*,#5080,.T.);
#6891=ORIENTED_EDGE('',*,*,#5079,.T.);
#6892=ORIENTED_EDGE('',*,*,#5081,.F.);
#6893=ORIENTED_EDGE('',*,*,#5082,.F.);
#6894=ORIENTED_EDGE('',*,*,#5083,.T.);
#6895=ORIENTED_EDGE('',*,*,#5082,.T.);
#6896=ORIENTED_EDGE('',*,*,#5084,.F.);
#6897=ORIENTED_EDGE('',*,*,#5085,.F.);
#6898=ORIENTED_EDGE('',*,*,#5086,.T.);
#6899=ORIENTED_EDGE('',*,*,#5085,.T.);
#6900=ORIENTED_EDGE('',*,*,#5087,.F.);
#6901=ORIENTED_EDGE('',*,*,#5088,.F.);
#6902=ORIENTED_EDGE('',*,*,#5089,.T.);
#6903=ORIENTED_EDGE('',*,*,#5088,.T.);
#6904=ORIENTED_EDGE('',*,*,#5090,.F.);
#6905=ORIENTED_EDGE('',*,*,#5091,.F.);
#6906=ORIENTED_EDGE('',*,*,#5092,.T.);
#6907=ORIENTED_EDGE('',*,*,#5091,.T.);
#6908=ORIENTED_EDGE('',*,*,#5093,.F.);
#6909=ORIENTED_EDGE('',*,*,#5094,.F.);
#6910=ORIENTED_EDGE('',*,*,#5095,.T.);
#6911=ORIENTED_EDGE('',*,*,#5094,.T.);
#6912=ORIENTED_EDGE('',*,*,#5096,.F.);
#6913=ORIENTED_EDGE('',*,*,#5097,.F.);
#6914=ORIENTED_EDGE('',*,*,#5098,.T.);
#6915=ORIENTED_EDGE('',*,*,#5097,.T.);
#6916=ORIENTED_EDGE('',*,*,#5099,.F.);
#6917=ORIENTED_EDGE('',*,*,#5077,.F.);
#6918=ORIENTED_EDGE('',*,*,#5099,.T.);
#6919=ORIENTED_EDGE('',*,*,#5096,.T.);
#6920=ORIENTED_EDGE('',*,*,#5093,.T.);
#6921=ORIENTED_EDGE('',*,*,#5090,.T.);
#6922=ORIENTED_EDGE('',*,*,#5087,.T.);
#6923=ORIENTED_EDGE('',*,*,#5084,.T.);
#6924=ORIENTED_EDGE('',*,*,#5081,.T.);
#6925=ORIENTED_EDGE('',*,*,#5078,.T.);
#6926=ORIENTED_EDGE('',*,*,#5098,.F.);
#6927=ORIENTED_EDGE('',*,*,#5076,.F.);
#6928=ORIENTED_EDGE('',*,*,#5080,.F.);
#6929=ORIENTED_EDGE('',*,*,#5083,.F.);
#6930=ORIENTED_EDGE('',*,*,#5086,.F.);
#6931=ORIENTED_EDGE('',*,*,#5089,.F.);
#6932=ORIENTED_EDGE('',*,*,#5092,.F.);
#6933=ORIENTED_EDGE('',*,*,#5095,.F.);
#6934=ORIENTED_EDGE('',*,*,#5100,.F.);
#6935=ORIENTED_EDGE('',*,*,#5101,.T.);
#6936=ORIENTED_EDGE('',*,*,#5102,.F.);
#6937=ORIENTED_EDGE('',*,*,#5103,.F.);
#6938=ORIENTED_EDGE('',*,*,#5104,.F.);
#6939=ORIENTED_EDGE('',*,*,#5103,.T.);
#6940=ORIENTED_EDGE('',*,*,#5105,.F.);
#6941=ORIENTED_EDGE('',*,*,#5106,.F.);
#6942=ORIENTED_EDGE('',*,*,#5107,.F.);
#6943=ORIENTED_EDGE('',*,*,#5106,.T.);
#6944=ORIENTED_EDGE('',*,*,#5108,.F.);
#6945=ORIENTED_EDGE('',*,*,#5109,.F.);
#6946=ORIENTED_EDGE('',*,*,#5110,.F.);
#6947=ORIENTED_EDGE('',*,*,#5109,.T.);
#6948=ORIENTED_EDGE('',*,*,#5111,.F.);
#6949=ORIENTED_EDGE('',*,*,#5112,.F.);
#6950=ORIENTED_EDGE('',*,*,#5113,.F.);
#6951=ORIENTED_EDGE('',*,*,#5112,.T.);
#6952=ORIENTED_EDGE('',*,*,#5114,.F.);
#6953=ORIENTED_EDGE('',*,*,#5115,.F.);
#6954=ORIENTED_EDGE('',*,*,#5116,.F.);
#6955=ORIENTED_EDGE('',*,*,#5115,.T.);
#6956=ORIENTED_EDGE('',*,*,#5117,.F.);
#6957=ORIENTED_EDGE('',*,*,#5118,.F.);
#6958=ORIENTED_EDGE('',*,*,#5119,.F.);
#6959=ORIENTED_EDGE('',*,*,#5118,.T.);
#6960=ORIENTED_EDGE('',*,*,#5120,.F.);
#6961=ORIENTED_EDGE('',*,*,#5121,.F.);
#6962=ORIENTED_EDGE('',*,*,#5122,.F.);
#6963=ORIENTED_EDGE('',*,*,#5121,.T.);
#6964=ORIENTED_EDGE('',*,*,#5123,.F.);
#6965=ORIENTED_EDGE('',*,*,#5101,.F.);
#6966=ORIENTED_EDGE('',*,*,#5122,.T.);
#6967=ORIENTED_EDGE('',*,*,#5100,.T.);
#6968=ORIENTED_EDGE('',*,*,#5104,.T.);
#6969=ORIENTED_EDGE('',*,*,#5107,.T.);
#6970=ORIENTED_EDGE('',*,*,#5110,.T.);
#6971=ORIENTED_EDGE('',*,*,#5113,.T.);
#6972=ORIENTED_EDGE('',*,*,#5116,.T.);
#6973=ORIENTED_EDGE('',*,*,#5119,.T.);
#6974=ORIENTED_EDGE('',*,*,#5123,.T.);
#6975=ORIENTED_EDGE('',*,*,#5120,.T.);
#6976=ORIENTED_EDGE('',*,*,#5117,.T.);
#6977=ORIENTED_EDGE('',*,*,#5114,.T.);
#6978=ORIENTED_EDGE('',*,*,#5111,.T.);
#6979=ORIENTED_EDGE('',*,*,#5108,.T.);
#6980=ORIENTED_EDGE('',*,*,#5105,.T.);
#6981=ORIENTED_EDGE('',*,*,#5102,.T.);
#6982=ORIENTED_EDGE('',*,*,#5124,.T.);
#6983=ORIENTED_EDGE('',*,*,#5125,.T.);
#6984=ORIENTED_EDGE('',*,*,#5126,.T.);
#6985=ORIENTED_EDGE('',*,*,#5127,.F.);
#6986=ORIENTED_EDGE('',*,*,#5128,.T.);
#6987=ORIENTED_EDGE('',*,*,#5129,.T.);
#6988=ORIENTED_EDGE('',*,*,#5130,.T.);
#6989=ORIENTED_EDGE('',*,*,#5125,.F.);
#6990=ORIENTED_EDGE('',*,*,#5131,.T.);
#6991=ORIENTED_EDGE('',*,*,#5132,.T.);
#6992=ORIENTED_EDGE('',*,*,#5133,.T.);
#6993=ORIENTED_EDGE('',*,*,#5129,.F.);
#6994=ORIENTED_EDGE('',*,*,#5134,.T.);
#6995=ORIENTED_EDGE('',*,*,#5135,.T.);
#6996=ORIENTED_EDGE('',*,*,#5136,.T.);
#6997=ORIENTED_EDGE('',*,*,#5132,.F.);
#6998=ORIENTED_EDGE('',*,*,#5137,.T.);
#6999=ORIENTED_EDGE('',*,*,#5138,.T.);
#7000=ORIENTED_EDGE('',*,*,#5139,.T.);
#7001=ORIENTED_EDGE('',*,*,#5135,.F.);
#7002=ORIENTED_EDGE('',*,*,#5140,.T.);
#7003=ORIENTED_EDGE('',*,*,#5127,.T.);
#7004=ORIENTED_EDGE('',*,*,#5141,.T.);
#7005=ORIENTED_EDGE('',*,*,#5138,.F.);
#7006=ORIENTED_EDGE('',*,*,#5140,.F.);
#7007=ORIENTED_EDGE('',*,*,#5137,.F.);
#7008=ORIENTED_EDGE('',*,*,#5134,.F.);
#7009=ORIENTED_EDGE('',*,*,#5131,.F.);
#7010=ORIENTED_EDGE('',*,*,#5128,.F.);
#7011=ORIENTED_EDGE('',*,*,#5124,.F.);
#7012=ORIENTED_EDGE('',*,*,#5141,.F.);
#7013=ORIENTED_EDGE('',*,*,#5126,.F.);
#7014=ORIENTED_EDGE('',*,*,#5130,.F.);
#7015=ORIENTED_EDGE('',*,*,#5133,.F.);
#7016=ORIENTED_EDGE('',*,*,#5136,.F.);
#7017=ORIENTED_EDGE('',*,*,#5139,.F.);
#7018=ORIENTED_EDGE('',*,*,#5142,.F.);
#7019=ORIENTED_EDGE('',*,*,#5143,.F.);
#7020=ORIENTED_EDGE('',*,*,#5144,.F.);
#7021=ORIENTED_EDGE('',*,*,#5145,.T.);
#7022=ORIENTED_EDGE('',*,*,#5143,.T.);
#7023=ORIENTED_EDGE('',*,*,#5145,.F.);
#7024=ORIENTED_EDGE('',*,*,#5146,.F.);
#7025=ORIENTED_EDGE('',*,*,#5147,.T.);
#7026=ORIENTED_EDGE('',*,*,#5144,.T.);
#7027=ORIENTED_EDGE('',*,*,#5147,.F.);
#7028=ORIENTED_EDGE('',*,*,#5148,.F.);
#7029=ORIENTED_EDGE('',*,*,#5149,.T.);
#7030=ORIENTED_EDGE('',*,*,#5146,.T.);
#7031=ORIENTED_EDGE('',*,*,#5149,.F.);
#7032=ORIENTED_EDGE('',*,*,#5148,.T.);
#7033=ORIENTED_EDGE('',*,*,#5150,.F.);
#7034=ORIENTED_EDGE('',*,*,#5151,.F.);
#7035=ORIENTED_EDGE('',*,*,#5152,.T.);
#7036=ORIENTED_EDGE('',*,*,#5150,.T.);
#7037=ORIENTED_EDGE('',*,*,#5152,.F.);
#7038=ORIENTED_EDGE('',*,*,#5142,.T.);
#7039=ORIENTED_EDGE('',*,*,#5153,.T.);
#7040=ORIENTED_EDGE('',*,*,#5151,.T.);
#7041=ORIENTED_EDGE('',*,*,#5153,.F.);
#7042=ORIENTED_EDGE('',*,*,#5154,.F.);
#7043=ORIENTED_EDGE('',*,*,#5155,.F.);
#7044=ORIENTED_EDGE('',*,*,#5156,.T.);
#7045=ORIENTED_EDGE('',*,*,#5154,.T.);
#7046=ORIENTED_EDGE('',*,*,#5156,.F.);
#7047=ORIENTED_EDGE('',*,*,#5157,.F.);
#7048=ORIENTED_EDGE('',*,*,#5158,.T.);
#7049=ORIENTED_EDGE('',*,*,#5155,.T.);
#7050=ORIENTED_EDGE('',*,*,#5158,.F.);
#7051=ORIENTED_EDGE('',*,*,#5159,.F.);
#7052=ORIENTED_EDGE('',*,*,#5160,.T.);
#7053=ORIENTED_EDGE('',*,*,#5157,.T.);
#7054=ORIENTED_EDGE('',*,*,#5160,.F.);
#7055=ORIENTED_EDGE('',*,*,#5159,.T.);
#7056=ORIENTED_EDGE('',*,*,#5161,.F.);
#7057=ORIENTED_EDGE('',*,*,#5162,.F.);
#7058=ORIENTED_EDGE('',*,*,#5163,.T.);
#7059=ORIENTED_EDGE('',*,*,#5161,.T.);
#7060=ORIENTED_EDGE('',*,*,#5163,.F.);
#7061=ORIENTED_EDGE('',*,*,#5164,.F.);
#7062=ORIENTED_EDGE('',*,*,#5165,.T.);
#7063=ORIENTED_EDGE('',*,*,#5162,.T.);
#7064=ORIENTED_EDGE('',*,*,#5165,.F.);
#7065=ORIENTED_EDGE('',*,*,#5166,.F.);
#7066=ORIENTED_EDGE('',*,*,#5167,.T.);
#7067=ORIENTED_EDGE('',*,*,#5164,.T.);
#7068=ORIENTED_EDGE('',*,*,#5167,.F.);
#7069=ORIENTED_EDGE('',*,*,#5166,.T.);
#7070=ORIENTED_EDGE('',*,*,#5168,.T.);
#7071=ORIENTED_EDGE('',*,*,#5169,.T.);
#7072=ORIENTED_EDGE('',*,*,#5170,.T.);
#7073=ORIENTED_EDGE('',*,*,#5171,.F.);
#7074=ORIENTED_EDGE('',*,*,#5172,.T.);
#7075=ORIENTED_EDGE('',*,*,#5173,.T.);
#7076=ORIENTED_EDGE('',*,*,#5174,.T.);
#7077=ORIENTED_EDGE('',*,*,#5169,.F.);
#7078=ORIENTED_EDGE('',*,*,#5175,.T.);
#7079=ORIENTED_EDGE('',*,*,#5176,.T.);
#7080=ORIENTED_EDGE('',*,*,#5177,.T.);
#7081=ORIENTED_EDGE('',*,*,#5173,.F.);
#7082=ORIENTED_EDGE('',*,*,#5178,.T.);
#7083=ORIENTED_EDGE('',*,*,#5179,.T.);
#7084=ORIENTED_EDGE('',*,*,#5180,.T.);
#7085=ORIENTED_EDGE('',*,*,#5176,.F.);
#7086=ORIENTED_EDGE('',*,*,#5181,.T.);
#7087=ORIENTED_EDGE('',*,*,#5182,.T.);
#7088=ORIENTED_EDGE('',*,*,#5183,.T.);
#7089=ORIENTED_EDGE('',*,*,#5179,.F.);
#7090=ORIENTED_EDGE('',*,*,#5184,.T.);
#7091=ORIENTED_EDGE('',*,*,#5171,.T.);
#7092=ORIENTED_EDGE('',*,*,#5185,.T.);
#7093=ORIENTED_EDGE('',*,*,#5182,.F.);
#7094=ORIENTED_EDGE('',*,*,#5184,.F.);
#7095=ORIENTED_EDGE('',*,*,#5181,.F.);
#7096=ORIENTED_EDGE('',*,*,#5178,.F.);
#7097=ORIENTED_EDGE('',*,*,#5175,.F.);
#7098=ORIENTED_EDGE('',*,*,#5172,.F.);
#7099=ORIENTED_EDGE('',*,*,#5168,.F.);
#7100=ORIENTED_EDGE('',*,*,#5185,.F.);
#7101=ORIENTED_EDGE('',*,*,#5170,.F.);
#7102=ORIENTED_EDGE('',*,*,#5174,.F.);
#7103=ORIENTED_EDGE('',*,*,#5177,.F.);
#7104=ORIENTED_EDGE('',*,*,#5180,.F.);
#7105=ORIENTED_EDGE('',*,*,#5183,.F.);
#7106=CYLINDRICAL_SURFACE('',#7989,0.274999999999999);
#7107=CYLINDRICAL_SURFACE('',#7992,0.275);
#7108=CYLINDRICAL_SURFACE('',#7995,0.275);
#7109=CYLINDRICAL_SURFACE('',#7998,0.274999999999999);
#7110=CYLINDRICAL_SURFACE('',#8008,0.274999999999999);
#7111=CYLINDRICAL_SURFACE('',#8011,0.275);
#7112=CYLINDRICAL_SURFACE('',#8014,0.275);
#7113=CYLINDRICAL_SURFACE('',#8017,0.274999999999999);
#7114=CYLINDRICAL_SURFACE('',#8052,0.225);
#7115=CYLINDRICAL_SURFACE('',#8055,0.225000000000001);
#7116=CYLINDRICAL_SURFACE('',#8065,0.225);
#7117=CYLINDRICAL_SURFACE('',#8068,0.225000000000001);
#7118=CYLINDRICAL_SURFACE('',#8078,0.165);
#7119=CYLINDRICAL_SURFACE('',#8082,0.5);
#7120=CYLINDRICAL_SURFACE('',#8087,0.275);
#7121=CYLINDRICAL_SURFACE('',#8096,0.165);
#7122=CYLINDRICAL_SURFACE('',#8100,0.5);
#7123=CYLINDRICAL_SURFACE('',#8105,0.275);
#7124=CYLINDRICAL_SURFACE('',#8114,0.164999999999999);
#7125=CYLINDRICAL_SURFACE('',#8118,0.5);
#7126=CYLINDRICAL_SURFACE('',#8123,0.274999999999999);
#7127=CYLINDRICAL_SURFACE('',#8132,0.164999999999999);
#7128=CYLINDRICAL_SURFACE('',#8136,0.5);
#7129=CYLINDRICAL_SURFACE('',#8141,0.274999999999999);
#7130=CYLINDRICAL_SURFACE('',#8172,0.210000000000001);
#7131=CYLINDRICAL_SURFACE('',#8175,0.21);
#7132=CYLINDRICAL_SURFACE('',#8178,0.164999999999999);
#7133=CYLINDRICAL_SURFACE('',#8181,0.164999999999999);
#7134=CYLINDRICAL_SURFACE('',#8184,0.164999999999999);
#7135=CYLINDRICAL_SURFACE('',#8187,0.164999999999999);
#7136=CYLINDRICAL_SURFACE('',#8190,0.275);
#7137=CYLINDRICAL_SURFACE('',#8193,0.274999999999999);
#7138=CYLINDRICAL_SURFACE('',#8203,0.225000000000001);
#7139=CYLINDRICAL_SURFACE('',#8206,0.225000000000001);
#7140=CYLINDRICAL_SURFACE('',#8218,0.164999999999999);
#7141=CYLINDRICAL_SURFACE('',#8222,0.274999999999999);
#7142=CYLINDRICAL_SURFACE('',#8235,0.164999999999999);
#7143=CYLINDRICAL_SURFACE('',#8239,0.274999999999999);
#7144=CYLINDRICAL_SURFACE('',#8252,0.275);
#7145=CYLINDRICAL_SURFACE('',#8262,0.274999999999999);
#7146=CYLINDRICAL_SURFACE('',#8308,0.21);
#7147=CYLINDRICAL_SURFACE('',#8326,0.425);
#7148=CYLINDRICAL_SURFACE('',#8334,0.24505);
#7149=CYLINDRICAL_SURFACE('',#8348,0.375);
#7150=CYLINDRICAL_SURFACE('',#8353,0.375);
#7151=CYLINDRICAL_SURFACE('',#8358,0.375);
#7152=CYLINDRICAL_SURFACE('',#8363,0.375);
#7153=CYLINDRICAL_SURFACE('',#8368,0.225);
#7154=CYLINDRICAL_SURFACE('',#8370,0.225);
#7155=CYLINDRICAL_SURFACE('',#8372,0.225);
#7156=CYLINDRICAL_SURFACE('',#8374,0.225000000000001);
#7157=CYLINDRICAL_SURFACE('',#8402,0.2117);
#7158=CYLINDRICAL_SURFACE('',#8415,0.265);
#7159=CYLINDRICAL_SURFACE('',#8419,0.5);
#7160=CYLINDRICAL_SURFACE('',#8434,0.25);
#7161=CYLINDRICAL_SURFACE('',#8441,0.425);
#7162=CYLINDRICAL_SURFACE('',#8449,0.24505);
#7163=CYLINDRICAL_SURFACE('',#8452,0.225);
#7164=CYLINDRICAL_SURFACE('',#8455,0.225);
#7165=CYLINDRICAL_SURFACE('',#8458,0.275);
#7166=CYLINDRICAL_SURFACE('',#8461,0.275);
#7167=CYLINDRICAL_SURFACE('',#8464,0.275);
#7168=CYLINDRICAL_SURFACE('',#8467,0.275);
#7169=CYLINDRICAL_SURFACE('',#8481,0.164999999999999);
#7170=CYLINDRICAL_SURFACE('',#8485,0.164999999999999);
#7171=CYLINDRICAL_SURFACE('',#8489,0.5);
#7172=CYLINDRICAL_SURFACE('',#8498,0.5);
#7173=CYLINDRICAL_SURFACE('',#8507,0.5);
#7174=CYLINDRICAL_SURFACE('',#8512,0.21);
#7175=CYLINDRICAL_SURFACE('',#8518,0.21);
#7176=CYLINDRICAL_SURFACE('',#8524,0.21);
#7177=CYLINDRICAL_SURFACE('',#8530,0.21);
#7178=CYLINDRICAL_SURFACE('',#8588,0.425);
#7179=CYLINDRICAL_SURFACE('',#8596,0.24505);
#7180=CYLINDRICAL_SURFACE('',#8602,0.35);
#7181=CYLINDRICAL_SURFACE('',#8610,0.1954);
#7182=ADVANCED_FACE('',(#914),#7106,.F.);
#7183=ADVANCED_FACE('',(#915),#7107,.F.);
#7184=ADVANCED_FACE('',(#916),#7108,.F.);
#7185=ADVANCED_FACE('',(#917),#7109,.F.);
#7186=ADVANCED_FACE('',(#918),#590,.T.);
#7187=ADVANCED_FACE('',(#919),#591,.T.);
#7188=ADVANCED_FACE('',(#920),#592,.T.);
#7189=ADVANCED_FACE('',(#921),#593,.T.);
#7190=ADVANCED_FACE('',(#922,#474,#475,#476,#477),#594,.T.);
#7191=ADVANCED_FACE('',(#923,#478,#479,#480,#481),#595,.F.);
#7192=ADVANCED_FACE('',(#924),#7110,.F.);
#7193=ADVANCED_FACE('',(#925),#7111,.F.);
#7194=ADVANCED_FACE('',(#926),#7112,.F.);
#7195=ADVANCED_FACE('',(#927),#7113,.F.);
#7196=ADVANCED_FACE('',(#928),#596,.F.);
#7197=ADVANCED_FACE('',(#929),#597,.F.);
#7198=ADVANCED_FACE('',(#930),#598,.F.);
#7199=ADVANCED_FACE('',(#931),#599,.F.);
#7200=ADVANCED_FACE('',(#932),#600,.T.);
#7201=ADVANCED_FACE('',(#933),#601,.T.);
#7202=ADVANCED_FACE('',(#934),#602,.T.);
#7203=ADVANCED_FACE('',(#935),#603,.T.);
#7204=ADVANCED_FACE('',(#936,#482,#483,#484,#485,#486),#604,.T.);
#7205=ADVANCED_FACE('',(#937,#487,#488,#489,#490,#491),#605,.F.);
#7206=ADVANCED_FACE('',(#938),#606,.T.);
#7207=ADVANCED_FACE('',(#939),#607,.T.);
#7208=ADVANCED_FACE('',(#940),#608,.T.);
#7209=ADVANCED_FACE('',(#941),#609,.T.);
#7210=ADVANCED_FACE('',(#942),#610,.T.);
#7211=ADVANCED_FACE('',(#943),#611,.F.);
#7212=ADVANCED_FACE('',(#944),#612,.T.);
#7213=ADVANCED_FACE('',(#945),#613,.T.);
#7214=ADVANCED_FACE('',(#946),#614,.T.);
#7215=ADVANCED_FACE('',(#947),#615,.T.);
#7216=ADVANCED_FACE('',(#948),#616,.T.);
#7217=ADVANCED_FACE('',(#949),#617,.F.);
#7218=ADVANCED_FACE('',(#950),#618,.T.);
#7219=ADVANCED_FACE('',(#951),#619,.T.);
#7220=ADVANCED_FACE('',(#952),#620,.T.);
#7221=ADVANCED_FACE('',(#953),#621,.T.);
#7222=ADVANCED_FACE('',(#954),#622,.T.);
#7223=ADVANCED_FACE('',(#955),#623,.F.);
#7224=ADVANCED_FACE('',(#956),#7114,.F.);
#7225=ADVANCED_FACE('',(#957),#7115,.F.);
#7226=ADVANCED_FACE('',(#958),#624,.T.);
#7227=ADVANCED_FACE('',(#959),#625,.T.);
#7228=ADVANCED_FACE('',(#960),#626,.T.);
#7229=ADVANCED_FACE('',(#961),#627,.T.);
#7230=ADVANCED_FACE('',(#962,#492,#493),#628,.T.);
#7231=ADVANCED_FACE('',(#963,#494,#495),#629,.F.);
#7232=ADVANCED_FACE('',(#964),#7116,.F.);
#7233=ADVANCED_FACE('',(#965),#7117,.F.);
#7234=ADVANCED_FACE('',(#966),#630,.T.);
#7235=ADVANCED_FACE('',(#967),#631,.T.);
#7236=ADVANCED_FACE('',(#968),#632,.T.);
#7237=ADVANCED_FACE('',(#969),#633,.T.);
#7238=ADVANCED_FACE('',(#970,#496,#497),#634,.T.);
#7239=ADVANCED_FACE('',(#971,#498,#499),#635,.F.);
#7240=ADVANCED_FACE('',(#972),#7118,.F.);
#7241=ADVANCED_FACE('',(#973),#636,.T.);
#7242=ADVANCED_FACE('',(#974),#7119,.F.);
#7243=ADVANCED_FACE('',(#975,#500),#637,.T.);
#7244=ADVANCED_FACE('',(#976),#7120,.F.);
#7245=ADVANCED_FACE('',(#977,#501,#502),#638,.T.);
#7246=ADVANCED_FACE('',(#978),#639,.T.);
#7247=ADVANCED_FACE('',(#979,#503),#640,.T.);
#7248=ADVANCED_FACE('',(#980),#641,.T.);
#7249=ADVANCED_FACE('',(#981),#642,.T.);
#7250=ADVANCED_FACE('',(#982),#643,.F.);
#7251=ADVANCED_FACE('',(#983),#7121,.F.);
#7252=ADVANCED_FACE('',(#984),#644,.F.);
#7253=ADVANCED_FACE('',(#985),#7122,.F.);
#7254=ADVANCED_FACE('',(#986,#504),#645,.F.);
#7255=ADVANCED_FACE('',(#987),#7123,.F.);
#7256=ADVANCED_FACE('',(#988,#505),#646,.T.);
#7257=ADVANCED_FACE('',(#989),#647,.T.);
#7258=ADVANCED_FACE('',(#990,#506,#507),#648,.T.);
#7259=ADVANCED_FACE('',(#991),#649,.T.);
#7260=ADVANCED_FACE('',(#992),#650,.T.);
#7261=ADVANCED_FACE('',(#993),#651,.F.);
#7262=ADVANCED_FACE('',(#994),#7124,.F.);
#7263=ADVANCED_FACE('',(#995),#652,.T.);
#7264=ADVANCED_FACE('',(#996),#7125,.F.);
#7265=ADVANCED_FACE('',(#997,#508),#653,.T.);
#7266=ADVANCED_FACE('',(#998),#7126,.F.);
#7267=ADVANCED_FACE('',(#999,#509,#510),#654,.T.);
#7268=ADVANCED_FACE('',(#1000),#655,.T.);
#7269=ADVANCED_FACE('',(#1001,#511),#656,.T.);
#7270=ADVANCED_FACE('',(#1002),#657,.T.);
#7271=ADVANCED_FACE('',(#1003),#658,.T.);
#7272=ADVANCED_FACE('',(#1004),#659,.F.);
#7273=ADVANCED_FACE('',(#1005),#7127,.F.);
#7274=ADVANCED_FACE('',(#1006),#660,.F.);
#7275=ADVANCED_FACE('',(#1007),#7128,.F.);
#7276=ADVANCED_FACE('',(#1008,#512),#661,.F.);
#7277=ADVANCED_FACE('',(#1009),#7129,.F.);
#7278=ADVANCED_FACE('',(#1010,#513),#662,.T.);
#7279=ADVANCED_FACE('',(#1011),#663,.T.);
#7280=ADVANCED_FACE('',(#1012,#514,#515),#664,.T.);
#7281=ADVANCED_FACE('',(#1013),#665,.T.);
#7282=ADVANCED_FACE('',(#1014),#666,.T.);
#7283=ADVANCED_FACE('',(#1015),#667,.F.);
#7284=ADVANCED_FACE('',(#1016),#668,.F.);
#7285=ADVANCED_FACE('',(#1017),#669,.F.);
#7286=ADVANCED_FACE('',(#1018),#670,.F.);
#7287=ADVANCED_FACE('',(#1019),#671,.F.);
#7288=ADVANCED_FACE('',(#1020),#672,.T.);
#7289=ADVANCED_FACE('',(#1021),#673,.T.);
#7290=ADVANCED_FACE('',(#1022),#674,.T.);
#7291=ADVANCED_FACE('',(#1023),#675,.T.);
#7292=ADVANCED_FACE('',(#1024,#516),#676,.T.);
#7293=ADVANCED_FACE('',(#1025,#517),#677,.F.);
#7294=ADVANCED_FACE('',(#1026),#678,.F.);
#7295=ADVANCED_FACE('',(#1027),#679,.F.);
#7296=ADVANCED_FACE('',(#1028),#680,.F.);
#7297=ADVANCED_FACE('',(#1029),#681,.F.);
#7298=ADVANCED_FACE('',(#1030),#682,.T.);
#7299=ADVANCED_FACE('',(#1031),#683,.T.);
#7300=ADVANCED_FACE('',(#1032),#684,.T.);
#7301=ADVANCED_FACE('',(#1033),#685,.T.);
#7302=ADVANCED_FACE('',(#1034,#518),#686,.T.);
#7303=ADVANCED_FACE('',(#1035,#519),#687,.F.);
#7304=ADVANCED_FACE('',(#1036),#7130,.F.);
#7305=ADVANCED_FACE('',(#1037),#7131,.F.);
#7306=ADVANCED_FACE('',(#1038),#7132,.F.);
#7307=ADVANCED_FACE('',(#1039),#7133,.F.);
#7308=ADVANCED_FACE('',(#1040),#7134,.F.);
#7309=ADVANCED_FACE('',(#1041),#7135,.F.);
#7310=ADVANCED_FACE('',(#1042),#7136,.F.);
#7311=ADVANCED_FACE('',(#1043),#7137,.F.);
#7312=ADVANCED_FACE('',(#1044),#688,.T.);
#7313=ADVANCED_FACE('',(#1045,#520,#521,#522,#523,#524,#525,#526,#527),
#689,.T.);
#7314=ADVANCED_FACE('',(#1046),#690,.T.);
#7315=ADVANCED_FACE('',(#1047,#528,#529,#530,#531,#532,#533,#534,#535),
#691,.T.);
#7316=ADVANCED_FACE('',(#1048),#692,.T.);
#7317=ADVANCED_FACE('',(#1049),#693,.F.);
#7318=ADVANCED_FACE('',(#1050),#7138,.F.);
#7319=ADVANCED_FACE('',(#1051),#7139,.F.);
#7320=ADVANCED_FACE('',(#1052),#694,.T.);
#7321=ADVANCED_FACE('',(#1053),#695,.T.);
#7322=ADVANCED_FACE('',(#1054),#696,.T.);
#7323=ADVANCED_FACE('',(#1055,#536,#537),#697,.T.);
#7324=ADVANCED_FACE('',(#1056),#698,.T.);
#7325=ADVANCED_FACE('',(#1057,#538,#539),#699,.T.);
#7326=ADVANCED_FACE('',(#1058),#700,.T.);
#7327=ADVANCED_FACE('',(#1059),#701,.F.);
#7328=ADVANCED_FACE('',(#1060),#7140,.F.);
#7329=ADVANCED_FACE('',(#1061),#702,.F.);
#7330=ADVANCED_FACE('',(#1062),#7141,.F.);
#7331=ADVANCED_FACE('',(#1063),#703,.T.);
#7332=ADVANCED_FACE('',(#1064,#540),#704,.T.);
#7333=ADVANCED_FACE('',(#1065),#705,.F.);
#7334=ADVANCED_FACE('',(#1066),#706,.T.);
#7335=ADVANCED_FACE('',(#1067),#707,.F.);
#7336=ADVANCED_FACE('',(#1068,#541),#708,.T.);
#7337=ADVANCED_FACE('',(#1069),#709,.T.);
#7338=ADVANCED_FACE('',(#1070,#542),#710,.T.);
#7339=ADVANCED_FACE('',(#1071),#711,.T.);
#7340=ADVANCED_FACE('',(#1072),#7142,.F.);
#7341=ADVANCED_FACE('',(#1073),#712,.F.);
#7342=ADVANCED_FACE('',(#1074),#7143,.F.);
#7343=ADVANCED_FACE('',(#1075),#713,.T.);
#7344=ADVANCED_FACE('',(#1076,#543),#714,.T.);
#7345=ADVANCED_FACE('',(#1077),#715,.F.);
#7346=ADVANCED_FACE('',(#1078),#716,.T.);
#7347=ADVANCED_FACE('',(#1079),#717,.F.);
#7348=ADVANCED_FACE('',(#1080,#544),#718,.T.);
#7349=ADVANCED_FACE('',(#1081),#719,.T.);
#7350=ADVANCED_FACE('',(#1082,#545),#720,.T.);
#7351=ADVANCED_FACE('',(#1083),#721,.T.);
#7352=ADVANCED_FACE('',(#1084),#7144,.F.);
#7353=ADVANCED_FACE('',(#1085),#722,.T.);
#7354=ADVANCED_FACE('',(#1086,#546),#723,.T.);
#7355=ADVANCED_FACE('',(#1087),#724,.T.);
#7356=ADVANCED_FACE('',(#1088,#547),#725,.T.);
#7357=ADVANCED_FACE('',(#1089),#726,.T.);
#7358=ADVANCED_FACE('',(#1090),#727,.F.);
#7359=ADVANCED_FACE('',(#1091),#7145,.F.);
#7360=ADVANCED_FACE('',(#1092),#728,.T.);
#7361=ADVANCED_FACE('',(#1093,#548),#729,.T.);
#7362=ADVANCED_FACE('',(#1094),#730,.T.);
#7363=ADVANCED_FACE('',(#1095,#549),#731,.T.);
#7364=ADVANCED_FACE('',(#1096),#732,.T.);
#7365=ADVANCED_FACE('',(#1097),#733,.F.);
#7366=ADVANCED_FACE('',(#1098),#734,.F.);
#7367=ADVANCED_FACE('',(#1099),#735,.F.);
#7368=ADVANCED_FACE('',(#1100),#736,.F.);
#7369=ADVANCED_FACE('',(#1101),#737,.F.);
#7370=ADVANCED_FACE('',(#1102),#738,.F.);
#7371=ADVANCED_FACE('',(#1103),#739,.F.);
#7372=ADVANCED_FACE('',(#1104),#740,.F.);
#7373=ADVANCED_FACE('',(#1105),#741,.F.);
#7374=ADVANCED_FACE('',(#1106),#742,.F.);
#7375=ADVANCED_FACE('',(#1107),#743,.F.);
#7376=ADVANCED_FACE('',(#1108),#744,.F.);
#7377=ADVANCED_FACE('',(#1109),#745,.F.);
#7378=ADVANCED_FACE('',(#1110),#746,.F.);
#7379=ADVANCED_FACE('',(#1111),#747,.F.);
#7380=ADVANCED_FACE('',(#1112),#748,.F.);
#7381=ADVANCED_FACE('',(#1113),#749,.F.);
#7382=ADVANCED_FACE('',(#1114),#750,.F.);
#7383=ADVANCED_FACE('',(#1115),#751,.F.);
#7384=ADVANCED_FACE('',(#1116),#752,.F.);
#7385=ADVANCED_FACE('',(#1117),#753,.F.);
#7386=ADVANCED_FACE('',(#1118),#754,.F.);
#7387=ADVANCED_FACE('',(#1119),#755,.F.);
#7388=ADVANCED_FACE('',(#1120),#756,.F.);
#7389=ADVANCED_FACE('',(#1121),#757,.F.);
#7390=ADVANCED_FACE('',(#1122),#758,.F.);
#7391=ADVANCED_FACE('',(#1123),#759,.F.);
#7392=ADVANCED_FACE('',(#1124),#760,.F.);
#7393=ADVANCED_FACE('',(#1125),#761,.F.);
#7394=ADVANCED_FACE('',(#1126),#762,.F.);
#7395=ADVANCED_FACE('',(#1127),#763,.F.);
#7396=ADVANCED_FACE('',(#1128),#764,.F.);
#7397=ADVANCED_FACE('',(#1129),#765,.F.);
#7398=ADVANCED_FACE('',(#1130),#766,.F.);
#7399=ADVANCED_FACE('',(#1131),#767,.F.);
#7400=ADVANCED_FACE('',(#1132),#768,.F.);
#7401=ADVANCED_FACE('',(#1133),#769,.F.);
#7402=ADVANCED_FACE('',(#1134),#7146,.F.);
#7403=ADVANCED_FACE('',(#1135),#770,.T.);
#7404=ADVANCED_FACE('',(#1136),#771,.T.);
#7405=ADVANCED_FACE('',(#1137),#772,.T.);
#7406=ADVANCED_FACE('',(#1138),#773,.T.);
#7407=ADVANCED_FACE('',(#1139),#774,.T.);
#7408=ADVANCED_FACE('',(#1140),#775,.T.);
#7409=ADVANCED_FACE('',(#1141),#776,.T.);
#7410=ADVANCED_FACE('',(#1142),#777,.T.);
#7411=ADVANCED_FACE('',(#1143,#550),#778,.T.);
#7412=ADVANCED_FACE('',(#1144,#551),#779,.F.);
#7413=ADVANCED_FACE('',(#1145),#780,.T.);
#7414=ADVANCED_FACE('',(#1146),#331,.T.);
#7415=ADVANCED_FACE('',(#1147),#7147,.T.);
#7416=ADVANCED_FACE('',(#1148),#332,.T.);
#7417=ADVANCED_FACE('',(#1149,#552),#781,.T.);
#7418=ADVANCED_FACE('',(#1150),#333,.T.);
#7419=ADVANCED_FACE('',(#1151),#7148,.T.);
#7420=ADVANCED_FACE('',(#1152),#334,.T.);
#7421=ADVANCED_FACE('',(#1153),#782,.T.);
#7422=ADVANCED_FACE('',(#1154),#783,.F.);
#7423=ADVANCED_FACE('',(#1155),#784,.F.);
#7424=ADVANCED_FACE('',(#1156),#785,.F.);
#7425=ADVANCED_FACE('',(#1157),#786,.F.);
#7426=ADVANCED_FACE('',(#1158),#787,.F.);
#7427=ADVANCED_FACE('',(#1159),#788,.F.);
#7428=ADVANCED_FACE('',(#1160),#789,.F.);
#7429=ADVANCED_FACE('',(#1161),#790,.F.);
#7430=ADVANCED_FACE('',(#1162),#7149,.F.);
#7431=ADVANCED_FACE('',(#1163,#553),#791,.T.);
#7432=ADVANCED_FACE('',(#1164),#7150,.F.);
#7433=ADVANCED_FACE('',(#1165,#554),#792,.T.);
#7434=ADVANCED_FACE('',(#1166),#7151,.F.);
#7435=ADVANCED_FACE('',(#1167,#555),#793,.T.);
#7436=ADVANCED_FACE('',(#1168),#7152,.F.);
#7437=ADVANCED_FACE('',(#1169,#556),#794,.T.);
#7438=ADVANCED_FACE('',(#1170),#7153,.F.);
#7439=ADVANCED_FACE('',(#1171),#7154,.F.);
#7440=ADVANCED_FACE('',(#1172),#7155,.F.);
#7441=ADVANCED_FACE('',(#1173),#7156,.F.);
#7442=ADVANCED_FACE('',(#1174),#795,.T.);
#7443=ADVANCED_FACE('',(#1175),#796,.T.);
#7444=ADVANCED_FACE('',(#1176),#797,.T.);
#7445=ADVANCED_FACE('',(#1177),#798,.T.);
#7446=ADVANCED_FACE('',(#1178,#557,#558,#559,#560),#799,.T.);
#7447=ADVANCED_FACE('',(#1179),#800,.T.);
#7448=ADVANCED_FACE('',(#1180),#801,.T.);
#7449=ADVANCED_FACE('',(#1181),#802,.T.);
#7450=ADVANCED_FACE('',(#1182),#803,.T.);
#7451=ADVANCED_FACE('',(#1183),#804,.T.);
#7452=ADVANCED_FACE('',(#1184,#561,#562,#563,#564),#805,.T.);
#7453=ADVANCED_FACE('',(#1185),#806,.T.);
#7454=ADVANCED_FACE('',(#1186),#807,.T.);
#7455=ADVANCED_FACE('',(#1187),#808,.F.);
#7456=ADVANCED_FACE('',(#1188),#809,.F.);
#7457=ADVANCED_FACE('',(#1189),#810,.T.);
#7458=ADVANCED_FACE('',(#1190,#565),#811,.T.);
#7459=ADVANCED_FACE('',(#1191),#812,.T.);
#7460=ADVANCED_FACE('',(#1192),#813,.T.);
#7461=ADVANCED_FACE('',(#1193),#814,.F.);
#7462=ADVANCED_FACE('',(#1194),#815,.T.);
#7463=ADVANCED_FACE('',(#1195),#816,.T.);
#7464=ADVANCED_FACE('',(#1196),#817,.T.);
#7465=ADVANCED_FACE('',(#1197),#7157,.F.);
#7466=ADVANCED_FACE('',(#1198),#818,.F.);
#7467=ADVANCED_FACE('',(#1199),#819,.F.);
#7468=ADVANCED_FACE('',(#1200),#820,.T.);
#7469=ADVANCED_FACE('',(#1201),#821,.T.);
#7470=ADVANCED_FACE('',(#1202),#335,.F.);
#7471=ADVANCED_FACE('',(#1203),#7158,.F.);
#7472=ADVANCED_FACE('',(#1204,#566),#822,.T.);
#7473=ADVANCED_FACE('',(#1205),#7159,.T.);
#7474=ADVANCED_FACE('',(#1206,#567),#823,.F.);
#7475=ADVANCED_FACE('',(#1207),#824,.F.);
#7476=ADVANCED_FACE('',(#1208),#825,.F.);
#7477=ADVANCED_FACE('',(#1209),#826,.F.);
#7478=ADVANCED_FACE('',(#1210),#827,.F.);
#7479=ADVANCED_FACE('',(#1211),#828,.F.);
#7480=ADVANCED_FACE('',(#1212),#829,.F.);
#7481=ADVANCED_FACE('',(#1213),#830,.F.);
#7482=ADVANCED_FACE('',(#1214),#831,.F.);
#7483=ADVANCED_FACE('',(#1215,#568),#832,.T.);
#7484=ADVANCED_FACE('',(#1216),#7160,.T.);
#7485=ADVANCED_FACE('',(#1217),#833,.F.);
#7486=ADVANCED_FACE('',(#1218),#834,.T.);
#7487=ADVANCED_FACE('',(#1219),#336,.T.);
#7488=ADVANCED_FACE('',(#1220),#7161,.T.);
#7489=ADVANCED_FACE('',(#1221),#337,.T.);
#7490=ADVANCED_FACE('',(#1222,#569),#835,.T.);
#7491=ADVANCED_FACE('',(#1223),#338,.T.);
#7492=ADVANCED_FACE('',(#1224),#7162,.T.);
#7493=ADVANCED_FACE('',(#1225),#7163,.F.);
#7494=ADVANCED_FACE('',(#1226),#7164,.F.);
#7495=ADVANCED_FACE('',(#1227),#7165,.F.);
#7496=ADVANCED_FACE('',(#1228),#7166,.F.);
#7497=ADVANCED_FACE('',(#1229),#7167,.F.);
#7498=ADVANCED_FACE('',(#1230),#7168,.F.);
#7499=ADVANCED_FACE('',(#1231),#836,.T.);
#7500=ADVANCED_FACE('',(#1232),#837,.T.);
#7501=ADVANCED_FACE('',(#1233),#838,.T.);
#7502=ADVANCED_FACE('',(#1234,#570,#571,#572,#573,#574,#575),#839,.F.);
#7503=ADVANCED_FACE('',(#1235),#840,.T.);
#7504=ADVANCED_FACE('',(#1236),#841,.T.);
#7505=ADVANCED_FACE('',(#1237),#842,.T.);
#7506=ADVANCED_FACE('',(#1238),#843,.T.);
#7507=ADVANCED_FACE('',(#1239),#844,.T.);
#7508=ADVANCED_FACE('',(#1240,#576,#577,#578,#579,#580,#581),#845,.T.);
#7509=ADVANCED_FACE('',(#1241),#7169,.F.);
#7510=ADVANCED_FACE('',(#1242),#846,.T.);
#7511=ADVANCED_FACE('',(#1243),#7170,.F.);
#7512=ADVANCED_FACE('',(#1244),#847,.T.);
#7513=ADVANCED_FACE('',(#1245),#7171,.T.);
#7514=ADVANCED_FACE('',(#1246,#582),#848,.T.);
#7515=ADVANCED_FACE('',(#1247),#849,.F.);
#7516=ADVANCED_FACE('',(#1248),#850,.T.);
#7517=ADVANCED_FACE('',(#1249),#7172,.T.);
#7518=ADVANCED_FACE('',(#1250,#583),#851,.T.);
#7519=ADVANCED_FACE('',(#1251),#852,.F.);
#7520=ADVANCED_FACE('',(#1252),#853,.F.);
#7521=ADVANCED_FACE('',(#1253),#7173,.T.);
#7522=ADVANCED_FACE('',(#1254),#854,.T.);
#7523=ADVANCED_FACE('',(#1255),#7174,.F.);
#7524=ADVANCED_FACE('',(#1256),#855,.T.);
#7525=ADVANCED_FACE('',(#1257),#7175,.F.);
#7526=ADVANCED_FACE('',(#1258),#856,.T.);
#7527=ADVANCED_FACE('',(#1259),#7176,.F.);
#7528=ADVANCED_FACE('',(#1260),#857,.T.);
#7529=ADVANCED_FACE('',(#1261),#7177,.F.);
#7530=ADVANCED_FACE('',(#1262),#858,.T.);
#7531=ADVANCED_FACE('',(#1263),#859,.T.);
#7532=ADVANCED_FACE('',(#1264),#860,.T.);
#7533=ADVANCED_FACE('',(#1265),#861,.T.);
#7534=ADVANCED_FACE('',(#1266),#862,.T.);
#7535=ADVANCED_FACE('',(#1267,#584,#585,#586,#587),#863,.T.);
#7536=ADVANCED_FACE('',(#1268),#864,.T.);
#7537=ADVANCED_FACE('',(#1269),#865,.T.);
#7538=ADVANCED_FACE('',(#1270),#866,.T.);
#7539=ADVANCED_FACE('',(#1271),#867,.T.);
#7540=ADVANCED_FACE('',(#1272),#868,.T.);
#7541=ADVANCED_FACE('',(#1273),#869,.T.);
#7542=ADVANCED_FACE('',(#1274),#870,.T.);
#7543=ADVANCED_FACE('',(#1275),#871,.T.);
#7544=ADVANCED_FACE('',(#1276),#872,.T.);
#7545=ADVANCED_FACE('',(#1277),#873,.T.);
#7546=ADVANCED_FACE('',(#1278),#874,.T.);
#7547=ADVANCED_FACE('',(#1279),#875,.T.);
#7548=ADVANCED_FACE('',(#1280),#876,.T.);
#7549=ADVANCED_FACE('',(#1281),#877,.T.);
#7550=ADVANCED_FACE('',(#1282),#878,.T.);
#7551=ADVANCED_FACE('',(#1283),#879,.T.);
#7552=ADVANCED_FACE('',(#1284),#880,.T.);
#7553=ADVANCED_FACE('',(#1285),#881,.F.);
#7554=ADVANCED_FACE('',(#1286),#882,.T.);
#7555=ADVANCED_FACE('',(#1287),#883,.T.);
#7556=ADVANCED_FACE('',(#1288),#884,.T.);
#7557=ADVANCED_FACE('',(#1289),#885,.T.);
#7558=ADVANCED_FACE('',(#1290),#886,.T.);
#7559=ADVANCED_FACE('',(#1291),#887,.T.);
#7560=ADVANCED_FACE('',(#1292),#888,.T.);
#7561=ADVANCED_FACE('',(#1293),#889,.T.);
#7562=ADVANCED_FACE('',(#1294),#890,.T.);
#7563=ADVANCED_FACE('',(#1295),#891,.T.);
#7564=ADVANCED_FACE('',(#1296),#892,.F.);
#7565=ADVANCED_FACE('',(#1297),#893,.F.);
#7566=ADVANCED_FACE('',(#1298),#894,.F.);
#7567=ADVANCED_FACE('',(#1299),#895,.F.);
#7568=ADVANCED_FACE('',(#1300),#896,.F.);
#7569=ADVANCED_FACE('',(#1301),#897,.F.);
#7570=ADVANCED_FACE('',(#1302),#898,.F.);
#7571=ADVANCED_FACE('',(#1303),#899,.F.);
#7572=ADVANCED_FACE('',(#1304),#900,.F.);
#7573=ADVANCED_FACE('',(#1305),#901,.T.);
#7574=ADVANCED_FACE('',(#1306),#339,.T.);
#7575=ADVANCED_FACE('',(#1307),#7178,.T.);
#7576=ADVANCED_FACE('',(#1308),#340,.T.);
#7577=ADVANCED_FACE('',(#1309,#588),#902,.T.);
#7578=ADVANCED_FACE('',(#1310),#341,.T.);
#7579=ADVANCED_FACE('',(#1311),#7179,.T.);
#7580=ADVANCED_FACE('',(#1312),#903,.T.);
#7581=ADVANCED_FACE('',(#1313),#342,.T.);
#7582=ADVANCED_FACE('',(#1314),#7180,.T.);
#7583=ADVANCED_FACE('',(#1315),#343,.T.);
#7584=ADVANCED_FACE('',(#1316,#589),#904,.T.);
#7585=ADVANCED_FACE('',(#1317),#344,.T.);
#7586=ADVANCED_FACE('',(#1318),#7181,.T.);
#7587=ADVANCED_FACE('',(#1319),#345,.T.);
#7588=ADVANCED_FACE('',(#1320),#905,.T.);
#7589=ADVANCED_FACE('',(#1321),#906,.F.);
#7590=ADVANCED_FACE('',(#1322),#907,.F.);
#7591=ADVANCED_FACE('',(#1323),#908,.F.);
#7592=ADVANCED_FACE('',(#1324),#909,.F.);
#7593=ADVANCED_FACE('',(#1325),#910,.F.);
#7594=ADVANCED_FACE('',(#1326),#911,.F.);
#7595=ADVANCED_FACE('',(#1327),#912,.F.);
#7596=ADVANCED_FACE('',(#1328),#913,.F.);
#7597=CLOSED_SHELL('',(#7182,#7183,#7184,#7185,#7186,#7187,#7188,#7189,
#7190,#7191));
#7598=CLOSED_SHELL('',(#7192,#7193,#7194,#7195,#7196,#7197,#7198,#7199,
#7200,#7201,#7202,#7203,#7204,#7205));
#7599=CLOSED_SHELL('',(#7206,#7207,#7208,#7209,#7210,#7211));
#7600=CLOSED_SHELL('',(#7212,#7213,#7214,#7215,#7216,#7217));
#7601=CLOSED_SHELL('',(#7218,#7219,#7220,#7221,#7222,#7223));
#7602=CLOSED_SHELL('',(#7224,#7225,#7226,#7227,#7228,#7229,#7230,#7231));
#7603=CLOSED_SHELL('',(#7232,#7233,#7234,#7235,#7236,#7237,#7238,#7239));
#7604=CLOSED_SHELL('',(#7240,#7241,#7242,#7243,#7244,#7245,#7246,#7247,
#7248,#7249,#7250));
#7605=CLOSED_SHELL('',(#7251,#7252,#7253,#7254,#7255,#7256,#7257,#7258,
#7259,#7260,#7261));
#7606=CLOSED_SHELL('',(#7262,#7263,#7264,#7265,#7266,#7267,#7268,#7269,
#7270,#7271,#7272));
#7607=CLOSED_SHELL('',(#7273,#7274,#7275,#7276,#7277,#7278,#7279,#7280,
#7281,#7282,#7283));
#7608=CLOSED_SHELL('',(#7284,#7285,#7286,#7287,#7288,#7289,#7290,#7291,
#7292,#7293));
#7609=CLOSED_SHELL('',(#7294,#7295,#7296,#7297,#7298,#7299,#7300,#7301,
#7302,#7303));
#7610=CLOSED_SHELL('',(#7304,#7305,#7306,#7307,#7308,#7309,#7310,#7311,
#7312,#7313,#7314,#7315,#7316,#7317));
#7611=CLOSED_SHELL('',(#7318,#7319,#7320,#7321,#7322,#7323,#7324,#7325,
#7326,#7327));
#7612=CLOSED_SHELL('',(#7328,#7329,#7330,#7331,#7332,#7333,#7334,#7335,
#7336,#7337,#7338,#7339));
#7613=CLOSED_SHELL('',(#7340,#7341,#7342,#7343,#7344,#7345,#7346,#7347,
#7348,#7349,#7350,#7351));
#7614=CLOSED_SHELL('',(#7352,#7353,#7354,#7355,#7356,#7357,#7358));
#7615=CLOSED_SHELL('',(#7359,#7360,#7361,#7362,#7363,#7364,#7365));
#7616=CLOSED_SHELL('',(#7366,#7367,#7368,#7369,#7370,#7371,#7372,#7373,
#7374,#7375,#7376,#7377,#7378,#7379,#7380,#7381,#7382,#7383,#7384,#7385,
#7386,#7387,#7388,#7389,#7390,#7391,#7392,#7393,#7394,#7395,#7396,#7397,
#7398,#7399,#7400,#7401,#7402,#7403,#7404,#7405,#7406,#7407,#7408,#7409,
#7410,#7411,#7412));
#7617=CLOSED_SHELL('',(#7413,#7414,#7415,#7416,#7417,#7418,#7419,#7420,
#7421));
#7618=CLOSED_SHELL('',(#7422,#7423,#7424,#7425,#7426,#7427,#7428,#7429));
#7619=CLOSED_SHELL('',(#7430,#7431,#7432,#7433,#7434,#7435,#7436,#7437,
#7438,#7439,#7440,#7441,#7442,#7443,#7444,#7445,#7446,#7447,#7448,#7449,
#7450,#7451,#7452,#7453,#7454,#7455));
#7620=CLOSED_SHELL('',(#7456,#7457,#7458,#7459,#7460,#7461,#7462,#7463,
#7464,#7465,#7466,#7467,#7468,#7469));
#7621=CLOSED_SHELL('',(#7470,#7471,#7472,#7473,#7474));
#7622=CLOSED_SHELL('',(#7475,#7476,#7477,#7478,#7479,#7480,#7481,#7482));
#7623=CLOSED_SHELL('',(#7483,#7484,#7485,#7486,#7487,#7488,#7489,#7490,
#7491,#7492));
#7624=CLOSED_SHELL('',(#7493,#7494,#7495,#7496,#7497,#7498,#7499,#7500,
#7501,#7502,#7503,#7504,#7505,#7506,#7507,#7508));
#7625=CLOSED_SHELL('',(#7509,#7510,#7511,#7512,#7513,#7514,#7515,#7516,
#7517,#7518,#7519,#7520,#7521));
#7626=CLOSED_SHELL('',(#7522,#7523,#7524,#7525,#7526,#7527,#7528,#7529,
#7530,#7531,#7532,#7533,#7534,#7535,#7536,#7537,#7538,#7539,#7540,#7541,
#7542,#7543));
#7627=CLOSED_SHELL('',(#7544,#7545,#7546,#7547,#7548,#7549,#7550,#7551,
#7552,#7553));
#7628=CLOSED_SHELL('',(#7554,#7555,#7556,#7557,#7558,#7559,#7560,#7561,
#7562,#7563));
#7629=CLOSED_SHELL('',(#7564,#7565,#7566,#7567,#7568,#7569,#7570,#7571));
#7630=CLOSED_SHELL('',(#7572,#7573,#7574,#7575,#7576,#7577,#7578,#7579));
#7631=CLOSED_SHELL('',(#7580,#7581,#7582,#7583,#7584,#7585,#7586,#7587,
#7588));
#7632=CLOSED_SHELL('',(#7589,#7590,#7591,#7592,#7593,#7594,#7595,#7596));
#7633=DERIVED_UNIT_ELEMENT(#7697,1.);
#7634=DERIVED_UNIT_ELEMENT(#13096,-3.);
#7635=DERIVED_UNIT_ELEMENT(#7697,1.);
#7636=DERIVED_UNIT_ELEMENT(#13096,-3.);
#7637=DERIVED_UNIT_ELEMENT(#7697,1.);
#7638=DERIVED_UNIT_ELEMENT(#13096,-3.);
#7639=DERIVED_UNIT_ELEMENT(#7697,1.);
#7640=DERIVED_UNIT_ELEMENT(#13096,-3.);
#7641=DERIVED_UNIT_ELEMENT(#7697,1.);
#7642=DERIVED_UNIT_ELEMENT(#13096,-3.);
#7643=DERIVED_UNIT_ELEMENT(#7697,1.);
#7644=DERIVED_UNIT_ELEMENT(#13096,-3.);
#7645=DERIVED_UNIT_ELEMENT(#7697,1.);
#7646=DERIVED_UNIT_ELEMENT(#13096,-3.);
#7647=DERIVED_UNIT_ELEMENT(#7697,1.);
#7648=DERIVED_UNIT_ELEMENT(#13096,-3.);
#7649=DERIVED_UNIT_ELEMENT(#7697,1.);
#7650=DERIVED_UNIT_ELEMENT(#13096,-3.);
#7651=DERIVED_UNIT_ELEMENT(#7697,1.);
#7652=DERIVED_UNIT_ELEMENT(#13096,-3.);
#7653=DERIVED_UNIT_ELEMENT(#7697,1.);
#7654=DERIVED_UNIT_ELEMENT(#13096,-3.);
#7655=DERIVED_UNIT_ELEMENT(#7697,1.);
#7656=DERIVED_UNIT_ELEMENT(#13096,-3.);
#7657=DERIVED_UNIT_ELEMENT(#7697,1.);
#7658=DERIVED_UNIT_ELEMENT(#13096,-3.);
#7659=DERIVED_UNIT_ELEMENT(#7697,1.);
#7660=DERIVED_UNIT_ELEMENT(#13096,-3.);
#7661=DERIVED_UNIT_ELEMENT(#7697,1.);
#7662=DERIVED_UNIT_ELEMENT(#13096,-3.);
#7663=DERIVED_UNIT_ELEMENT(#7697,1.);
#7664=DERIVED_UNIT_ELEMENT(#13096,-3.);
#7665=DERIVED_UNIT_ELEMENT(#7697,1.);
#7666=DERIVED_UNIT_ELEMENT(#13096,-3.);
#7667=DERIVED_UNIT_ELEMENT(#7697,1.);
#7668=DERIVED_UNIT_ELEMENT(#13096,-3.);
#7669=DERIVED_UNIT_ELEMENT(#7697,1.);
#7670=DERIVED_UNIT_ELEMENT(#13096,-3.);
#7671=DERIVED_UNIT_ELEMENT(#7697,1.);
#7672=DERIVED_UNIT_ELEMENT(#13096,-3.);
#7673=DERIVED_UNIT_ELEMENT(#7697,1.);
#7674=DERIVED_UNIT_ELEMENT(#13096,-3.);
#7675=DERIVED_UNIT_ELEMENT(#7697,1.);
#7676=DERIVED_UNIT_ELEMENT(#13096,-3.);
#7677=DERIVED_UNIT_ELEMENT(#7697,1.);
#7678=DERIVED_UNIT_ELEMENT(#13096,-3.);
#7679=DERIVED_UNIT_ELEMENT(#7697,1.);
#7680=DERIVED_UNIT_ELEMENT(#13096,-3.);
#7681=DERIVED_UNIT_ELEMENT(#7697,1.);
#7682=DERIVED_UNIT_ELEMENT(#13096,-3.);
#7683=DERIVED_UNIT_ELEMENT(#7697,1.);
#7684=DERIVED_UNIT_ELEMENT(#13096,-3.);
#7685=DERIVED_UNIT_ELEMENT(#7697,1.);
#7686=DERIVED_UNIT_ELEMENT(#13096,-3.);
#7687=DERIVED_UNIT_ELEMENT(#7697,1.);
#7688=DERIVED_UNIT_ELEMENT(#13096,-3.);
#7689=DERIVED_UNIT_ELEMENT(#7697,1.);
#7690=DERIVED_UNIT_ELEMENT(#13096,-3.);
#7691=DERIVED_UNIT_ELEMENT(#7697,1.);
#7692=DERIVED_UNIT_ELEMENT(#13096,-3.);
#7693=DERIVED_UNIT_ELEMENT(#7697,1.);
#7694=DERIVED_UNIT_ELEMENT(#13096,-3.);
#7695=DERIVED_UNIT_ELEMENT(#7697,1.);
#7696=DERIVED_UNIT_ELEMENT(#13096,-3.);
#7697=(
MASS_UNIT()
NAMED_UNIT(*)
SI_UNIT(.KILO.,.GRAM.)
);
#7698=DERIVED_UNIT((#7633,#7634));
#7699=DERIVED_UNIT((#7635,#7636));
#7700=DERIVED_UNIT((#7637,#7638));
#7701=DERIVED_UNIT((#7639,#7640));
#7702=DERIVED_UNIT((#7641,#7642));
#7703=DERIVED_UNIT((#7643,#7644));
#7704=DERIVED_UNIT((#7645,#7646));
#7705=DERIVED_UNIT((#7647,#7648));
#7706=DERIVED_UNIT((#7649,#7650));
#7707=DERIVED_UNIT((#7651,#7652));
#7708=DERIVED_UNIT((#7653,#7654));
#7709=DERIVED_UNIT((#7655,#7656));
#7710=DERIVED_UNIT((#7657,#7658));
#7711=DERIVED_UNIT((#7659,#7660));
#7712=DERIVED_UNIT((#7661,#7662));
#7713=DERIVED_UNIT((#7663,#7664));
#7714=DERIVED_UNIT((#7665,#7666));
#7715=DERIVED_UNIT((#7667,#7668));
#7716=DERIVED_UNIT((#7669,#7670));
#7717=DERIVED_UNIT((#7671,#7672));
#7718=DERIVED_UNIT((#7673,#7674));
#7719=DERIVED_UNIT((#7675,#7676));
#7720=DERIVED_UNIT((#7677,#7678));
#7721=DERIVED_UNIT((#7679,#7680));
#7722=DERIVED_UNIT((#7681,#7682));
#7723=DERIVED_UNIT((#7683,#7684));
#7724=DERIVED_UNIT((#7685,#7686));
#7725=DERIVED_UNIT((#7687,#7688));
#7726=DERIVED_UNIT((#7689,#7690));
#7727=DERIVED_UNIT((#7691,#7692));
#7728=DERIVED_UNIT((#7693,#7694));
#7729=DERIVED_UNIT((#7695,#7696));
#7730=MEASURE_REPRESENTATION_ITEM('density measure',
POSITIVE_RATIO_MEASURE(7850.),#7698);
#7731=MEASURE_REPRESENTATION_ITEM('density measure',
POSITIVE_RATIO_MEASURE(7850.),#7699);
#7732=MEASURE_REPRESENTATION_ITEM('density measure',
POSITIVE_RATIO_MEASURE(7850.),#7700);
#7733=MEASURE_REPRESENTATION_ITEM('density measure',
POSITIVE_RATIO_MEASURE(7850.),#7701);
#7734=MEASURE_REPRESENTATION_ITEM('density measure',
POSITIVE_RATIO_MEASURE(7850.),#7702);
#7735=MEASURE_REPRESENTATION_ITEM('density measure',
POSITIVE_RATIO_MEASURE(7850.),#7703);
#7736=MEASURE_REPRESENTATION_ITEM('density measure',
POSITIVE_RATIO_MEASURE(7850.),#7704);
#7737=MEASURE_REPRESENTATION_ITEM('density measure',
POSITIVE_RATIO_MEASURE(7850.),#7705);
#7738=MEASURE_REPRESENTATION_ITEM('density measure',
POSITIVE_RATIO_MEASURE(7850.),#7706);
#7739=MEASURE_REPRESENTATION_ITEM('density measure',
POSITIVE_RATIO_MEASURE(7850.),#7707);
#7740=MEASURE_REPRESENTATION_ITEM('density measure',
POSITIVE_RATIO_MEASURE(7850.),#7708);
#7741=MEASURE_REPRESENTATION_ITEM('density measure',
POSITIVE_RATIO_MEASURE(7850.),#7709);
#7742=MEASURE_REPRESENTATION_ITEM('density measure',
POSITIVE_RATIO_MEASURE(7850.),#7710);
#7743=MEASURE_REPRESENTATION_ITEM('density measure',
POSITIVE_RATIO_MEASURE(7850.),#7711);
#7744=MEASURE_REPRESENTATION_ITEM('density measure',
POSITIVE_RATIO_MEASURE(7850.),#7712);
#7745=MEASURE_REPRESENTATION_ITEM('density measure',
POSITIVE_RATIO_MEASURE(7850.),#7713);
#7746=MEASURE_REPRESENTATION_ITEM('density measure',
POSITIVE_RATIO_MEASURE(7850.),#7714);
#7747=MEASURE_REPRESENTATION_ITEM('density measure',
POSITIVE_RATIO_MEASURE(7850.),#7715);
#7748=MEASURE_REPRESENTATION_ITEM('density measure',
POSITIVE_RATIO_MEASURE(7850.),#7716);
#7749=MEASURE_REPRESENTATION_ITEM('density measure',
POSITIVE_RATIO_MEASURE(7850.),#7717);
#7750=MEASURE_REPRESENTATION_ITEM('density measure',
POSITIVE_RATIO_MEASURE(7850.),#7718);
#7751=MEASURE_REPRESENTATION_ITEM('density measure',
POSITIVE_RATIO_MEASURE(7850.),#7719);
#7752=MEASURE_REPRESENTATION_ITEM('density measure',
POSITIVE_RATIO_MEASURE(7850.),#7720);
#7753=MEASURE_REPRESENTATION_ITEM('density measure',
POSITIVE_RATIO_MEASURE(7850.),#7721);
#7754=MEASURE_REPRESENTATION_ITEM('density measure',
POSITIVE_RATIO_MEASURE(7850.),#7722);
#7755=MEASURE_REPRESENTATION_ITEM('density measure',
POSITIVE_RATIO_MEASURE(7850.),#7723);
#7756=MEASURE_REPRESENTATION_ITEM('density measure',
POSITIVE_RATIO_MEASURE(7850.),#7724);
#7757=MEASURE_REPRESENTATION_ITEM('density measure',
POSITIVE_RATIO_MEASURE(7850.),#7725);
#7758=MEASURE_REPRESENTATION_ITEM('density measure',
POSITIVE_RATIO_MEASURE(7850.),#7726);
#7759=MEASURE_REPRESENTATION_ITEM('density measure',
POSITIVE_RATIO_MEASURE(7850.),#7727);
#7760=MEASURE_REPRESENTATION_ITEM('density measure',
POSITIVE_RATIO_MEASURE(7850.),#7728);
#7761=MEASURE_REPRESENTATION_ITEM('density measure',
POSITIVE_RATIO_MEASURE(7850.),#7729);
#7762=PROPERTY_DEFINITION_REPRESENTATION(#7922,#7826);
#7763=PROPERTY_DEFINITION_REPRESENTATION(#7923,#7827);
#7764=PROPERTY_DEFINITION_REPRESENTATION(#7924,#7828);
#7765=PROPERTY_DEFINITION_REPRESENTATION(#7925,#7829);
#7766=PROPERTY_DEFINITION_REPRESENTATION(#7926,#7830);
#7767=PROPERTY_DEFINITION_REPRESENTATION(#7927,#7831);
#7768=PROPERTY_DEFINITION_REPRESENTATION(#7928,#7832);
#7769=PROPERTY_DEFINITION_REPRESENTATION(#7929,#7833);
#7770=PROPERTY_DEFINITION_REPRESENTATION(#7930,#7834);
#7771=PROPERTY_DEFINITION_REPRESENTATION(#7931,#7835);
#7772=PROPERTY_DEFINITION_REPRESENTATION(#7932,#7836);
#7773=PROPERTY_DEFINITION_REPRESENTATION(#7933,#7837);
#7774=PROPERTY_DEFINITION_REPRESENTATION(#7934,#7838);
#7775=PROPERTY_DEFINITION_REPRESENTATION(#7935,#7839);
#7776=PROPERTY_DEFINITION_REPRESENTATION(#7936,#7840);
#7777=PROPERTY_DEFINITION_REPRESENTATION(#7937,#7841);
#7778=PROPERTY_DEFINITION_REPRESENTATION(#7938,#7842);
#7779=PROPERTY_DEFINITION_REPRESENTATION(#7939,#7843);
#7780=PROPERTY_DEFINITION_REPRESENTATION(#7940,#7844);
#7781=PROPERTY_DEFINITION_REPRESENTATION(#7941,#7845);
#7782=PROPERTY_DEFINITION_REPRESENTATION(#7942,#7846);
#7783=PROPERTY_DEFINITION_REPRESENTATION(#7943,#7847);
#7784=PROPERTY_DEFINITION_REPRESENTATION(#7944,#7848);
#7785=PROPERTY_DEFINITION_REPRESENTATION(#7945,#7849);
#7786=PROPERTY_DEFINITION_REPRESENTATION(#7946,#7850);
#7787=PROPERTY_DEFINITION_REPRESENTATION(#7947,#7851);
#7788=PROPERTY_DEFINITION_REPRESENTATION(#7948,#7852);
#7789=PROPERTY_DEFINITION_REPRESENTATION(#7949,#7853);
#7790=PROPERTY_DEFINITION_REPRESENTATION(#7950,#7854);
#7791=PROPERTY_DEFINITION_REPRESENTATION(#7951,#7855);
#7792=PROPERTY_DEFINITION_REPRESENTATION(#7952,#7856);
#7793=PROPERTY_DEFINITION_REPRESENTATION(#7953,#7857);
#7794=PROPERTY_DEFINITION_REPRESENTATION(#7954,#7858);
#7795=PROPERTY_DEFINITION_REPRESENTATION(#7955,#7859);
#7796=PROPERTY_DEFINITION_REPRESENTATION(#7956,#7860);
#7797=PROPERTY_DEFINITION_REPRESENTATION(#7957,#7861);
#7798=PROPERTY_DEFINITION_REPRESENTATION(#7958,#7862);
#7799=PROPERTY_DEFINITION_REPRESENTATION(#7959,#7863);
#7800=PROPERTY_DEFINITION_REPRESENTATION(#7960,#7864);
#7801=PROPERTY_DEFINITION_REPRESENTATION(#7961,#7865);
#7802=PROPERTY_DEFINITION_REPRESENTATION(#7962,#7866);
#7803=PROPERTY_DEFINITION_REPRESENTATION(#7963,#7867);
#7804=PROPERTY_DEFINITION_REPRESENTATION(#7964,#7868);
#7805=PROPERTY_DEFINITION_REPRESENTATION(#7965,#7869);
#7806=PROPERTY_DEFINITION_REPRESENTATION(#7966,#7870);
#7807=PROPERTY_DEFINITION_REPRESENTATION(#7967,#7871);
#7808=PROPERTY_DEFINITION_REPRESENTATION(#7968,#7872);
#7809=PROPERTY_DEFINITION_REPRESENTATION(#7969,#7873);
#7810=PROPERTY_DEFINITION_REPRESENTATION(#7970,#7874);
#7811=PROPERTY_DEFINITION_REPRESENTATION(#7971,#7875);
#7812=PROPERTY_DEFINITION_REPRESENTATION(#7972,#7876);
#7813=PROPERTY_DEFINITION_REPRESENTATION(#7973,#7877);
#7814=PROPERTY_DEFINITION_REPRESENTATION(#7974,#7878);
#7815=PROPERTY_DEFINITION_REPRESENTATION(#7975,#7879);
#7816=PROPERTY_DEFINITION_REPRESENTATION(#7976,#7880);
#7817=PROPERTY_DEFINITION_REPRESENTATION(#7977,#7881);
#7818=PROPERTY_DEFINITION_REPRESENTATION(#7978,#7882);
#7819=PROPERTY_DEFINITION_REPRESENTATION(#7979,#7883);
#7820=PROPERTY_DEFINITION_REPRESENTATION(#7980,#7884);
#7821=PROPERTY_DEFINITION_REPRESENTATION(#7981,#7885);
#7822=PROPERTY_DEFINITION_REPRESENTATION(#7982,#7886);
#7823=PROPERTY_DEFINITION_REPRESENTATION(#7983,#7887);
#7824=PROPERTY_DEFINITION_REPRESENTATION(#7984,#7888);
#7825=PROPERTY_DEFINITION_REPRESENTATION(#7985,#7889);
#7826=REPRESENTATION('material name',(#7890),#13060);
#7827=REPRESENTATION('density',(#7730),#13060);
#7828=REPRESENTATION('material name',(#7891),#13061);
#7829=REPRESENTATION('density',(#7731),#13061);
#7830=REPRESENTATION('material name',(#7892),#13062);
#7831=REPRESENTATION('density',(#7732),#13062);
#7832=REPRESENTATION('material name',(#7893),#13063);
#7833=REPRESENTATION('density',(#7733),#13063);
#7834=REPRESENTATION('material name',(#7894),#13064);
#7835=REPRESENTATION('density',(#7734),#13064);
#7836=REPRESENTATION('material name',(#7895),#13065);
#7837=REPRESENTATION('density',(#7735),#13065);
#7838=REPRESENTATION('material name',(#7896),#13066);
#7839=REPRESENTATION('density',(#7736),#13066);
#7840=REPRESENTATION('material name',(#7897),#13067);
#7841=REPRESENTATION('density',(#7737),#13067);
#7842=REPRESENTATION('material name',(#7898),#13068);
#7843=REPRESENTATION('density',(#7738),#13068);
#7844=REPRESENTATION('material name',(#7899),#13069);
#7845=REPRESENTATION('density',(#7739),#13069);
#7846=REPRESENTATION('material name',(#7900),#13070);
#7847=REPRESENTATION('density',(#7740),#13070);
#7848=REPRESENTATION('material name',(#7901),#13071);
#7849=REPRESENTATION('density',(#7741),#13071);
#7850=REPRESENTATION('material name',(#7902),#13072);
#7851=REPRESENTATION('density',(#7742),#13072);
#7852=REPRESENTATION('material name',(#7903),#13073);
#7853=REPRESENTATION('density',(#7743),#13073);
#7854=REPRESENTATION('material name',(#7904),#13074);
#7855=REPRESENTATION('density',(#7744),#13074);
#7856=REPRESENTATION('material name',(#7905),#13075);
#7857=REPRESENTATION('density',(#7745),#13075);
#7858=REPRESENTATION('material name',(#7906),#13076);
#7859=REPRESENTATION('density',(#7746),#13076);
#7860=REPRESENTATION('material name',(#7907),#13077);
#7861=REPRESENTATION('density',(#7747),#13077);
#7862=REPRESENTATION('material name',(#7908),#13078);
#7863=REPRESENTATION('density',(#7748),#13078);
#7864=REPRESENTATION('material name',(#7909),#13079);
#7865=REPRESENTATION('density',(#7749),#13079);
#7866=REPRESENTATION('material name',(#7910),#13080);
#7867=REPRESENTATION('density',(#7750),#13080);
#7868=REPRESENTATION('material name',(#7911),#13081);
#7869=REPRESENTATION('density',(#7751),#13081);
#7870=REPRESENTATION('material name',(#7912),#13082);
#7871=REPRESENTATION('density',(#7752),#13082);
#7872=REPRESENTATION('material name',(#7913),#13083);
#7873=REPRESENTATION('density',(#7753),#13083);
#7874=REPRESENTATION('material name',(#7914),#13084);
#7875=REPRESENTATION('density',(#7754),#13084);
#7876=REPRESENTATION('material name',(#7915),#13086);
#7877=REPRESENTATION('density',(#7755),#13086);
#7878=REPRESENTATION('material name',(#7916),#13087);
#7879=REPRESENTATION('density',(#7756),#13087);
#7880=REPRESENTATION('material name',(#7917),#13089);
#7881=REPRESENTATION('density',(#7757),#13089);
#7882=REPRESENTATION('material name',(#7918),#13090);
#7883=REPRESENTATION('density',(#7758),#13090);
#7884=REPRESENTATION('material name',(#7919),#13091);
#7885=REPRESENTATION('density',(#7759),#13091);
#7886=REPRESENTATION('material name',(#7920),#13092);
#7887=REPRESENTATION('density',(#7760),#13092);
#7888=REPRESENTATION('material name',(#7921),#13093);
#7889=REPRESENTATION('density',(#7761),#13093);
#7890=DESCRIPTIVE_REPRESENTATION_ITEM('Steel','Steel');
#7891=DESCRIPTIVE_REPRESENTATION_ITEM('Steel','Steel');
#7892=DESCRIPTIVE_REPRESENTATION_ITEM('Steel','Steel');
#7893=DESCRIPTIVE_REPRESENTATION_ITEM('Steel','Steel');
#7894=DESCRIPTIVE_REPRESENTATION_ITEM('Steel','Steel');
#7895=DESCRIPTIVE_REPRESENTATION_ITEM('Steel','Steel');
#7896=DESCRIPTIVE_REPRESENTATION_ITEM('Steel','Steel');
#7897=DESCRIPTIVE_REPRESENTATION_ITEM('Steel','Steel');
#7898=DESCRIPTIVE_REPRESENTATION_ITEM('Steel','Steel');
#7899=DESCRIPTIVE_REPRESENTATION_ITEM('Steel','Steel');
#7900=DESCRIPTIVE_REPRESENTATION_ITEM('Steel','Steel');
#7901=DESCRIPTIVE_REPRESENTATION_ITEM('Steel','Steel');
#7902=DESCRIPTIVE_REPRESENTATION_ITEM('Steel','Steel');
#7903=DESCRIPTIVE_REPRESENTATION_ITEM('Steel','Steel');
#7904=DESCRIPTIVE_REPRESENTATION_ITEM('Steel','Steel');
#7905=DESCRIPTIVE_REPRESENTATION_ITEM('Steel','Steel');
#7906=DESCRIPTIVE_REPRESENTATION_ITEM('Steel','Steel');
#7907=DESCRIPTIVE_REPRESENTATION_ITEM('Steel','Steel');
#7908=DESCRIPTIVE_REPRESENTATION_ITEM('Steel','Steel');
#7909=DESCRIPTIVE_REPRESENTATION_ITEM('Steel','Steel');
#7910=DESCRIPTIVE_REPRESENTATION_ITEM('Steel','Steel');
#7911=DESCRIPTIVE_REPRESENTATION_ITEM('Steel','Steel');
#7912=DESCRIPTIVE_REPRESENTATION_ITEM('Steel','Steel');
#7913=DESCRIPTIVE_REPRESENTATION_ITEM('Steel','Steel');
#7914=DESCRIPTIVE_REPRESENTATION_ITEM('Steel','Steel');
#7915=DESCRIPTIVE_REPRESENTATION_ITEM('Steel','Steel');
#7916=DESCRIPTIVE_REPRESENTATION_ITEM('Steel','Steel');
#7917=DESCRIPTIVE_REPRESENTATION_ITEM('Steel','Steel');
#7918=DESCRIPTIVE_REPRESENTATION_ITEM('Steel','Steel');
#7919=DESCRIPTIVE_REPRESENTATION_ITEM('Steel','Steel');
#7920=DESCRIPTIVE_REPRESENTATION_ITEM('Steel','Steel');
#7921=DESCRIPTIVE_REPRESENTATION_ITEM('Steel','Steel');
#7922=PROPERTY_DEFINITION('material property','material name',#13288);
#7923=PROPERTY_DEFINITION('material property','density of part',#13288);
#7924=PROPERTY_DEFINITION('material property','material name',#13289);
#7925=PROPERTY_DEFINITION('material property','density of part',#13289);
#7926=PROPERTY_DEFINITION('material property','material name',#13290);
#7927=PROPERTY_DEFINITION('material property','density of part',#13290);
#7928=PROPERTY_DEFINITION('material property','material name',#13291);
#7929=PROPERTY_DEFINITION('material property','density of part',#13291);
#7930=PROPERTY_DEFINITION('material property','material name',#13292);
#7931=PROPERTY_DEFINITION('material property','density of part',#13292);
#7932=PROPERTY_DEFINITION('material property','material name',#13293);
#7933=PROPERTY_DEFINITION('material property','density of part',#13293);
#7934=PROPERTY_DEFINITION('material property','material name',#13294);
#7935=PROPERTY_DEFINITION('material property','density of part',#13294);
#7936=PROPERTY_DEFINITION('material property','material name',#13295);
#7937=PROPERTY_DEFINITION('material property','density of part',#13295);
#7938=PROPERTY_DEFINITION('material property','material name',#13296);
#7939=PROPERTY_DEFINITION('material property','density of part',#13296);
#7940=PROPERTY_DEFINITION('material property','material name',#13297);
#7941=PROPERTY_DEFINITION('material property','density of part',#13297);
#7942=PROPERTY_DEFINITION('material property','material name',#13298);
#7943=PROPERTY_DEFINITION('material property','density of part',#13298);
#7944=PROPERTY_DEFINITION('material property','material name',#13299);
#7945=PROPERTY_DEFINITION('material property','density of part',#13299);
#7946=PROPERTY_DEFINITION('material property','material name',#13300);
#7947=PROPERTY_DEFINITION('material property','density of part',#13300);
#7948=PROPERTY_DEFINITION('material property','material name',#13301);
#7949=PROPERTY_DEFINITION('material property','density of part',#13301);
#7950=PROPERTY_DEFINITION('material property','material name',#13302);
#7951=PROPERTY_DEFINITION('material property','density of part',#13302);
#7952=PROPERTY_DEFINITION('material property','material name',#13303);
#7953=PROPERTY_DEFINITION('material property','density of part',#13303);
#7954=PROPERTY_DEFINITION('material property','material name',#13304);
#7955=PROPERTY_DEFINITION('material property','density of part',#13304);
#7956=PROPERTY_DEFINITION('material property','material name',#13305);
#7957=PROPERTY_DEFINITION('material property','density of part',#13305);
#7958=PROPERTY_DEFINITION('material property','material name',#13306);
#7959=PROPERTY_DEFINITION('material property','density of part',#13306);
#7960=PROPERTY_DEFINITION('material property','material name',#13307);
#7961=PROPERTY_DEFINITION('material property','density of part',#13307);
#7962=PROPERTY_DEFINITION('material property','material name',#13308);
#7963=PROPERTY_DEFINITION('material property','density of part',#13308);
#7964=PROPERTY_DEFINITION('material property','material name',#13309);
#7965=PROPERTY_DEFINITION('material property','density of part',#13309);
#7966=PROPERTY_DEFINITION('material property','material name',#13310);
#7967=PROPERTY_DEFINITION('material property','density of part',#13310);
#7968=PROPERTY_DEFINITION('material property','material name',#13311);
#7969=PROPERTY_DEFINITION('material property','density of part',#13311);
#7970=PROPERTY_DEFINITION('material property','material name',#13312);
#7971=PROPERTY_DEFINITION('material property','density of part',#13312);
#7972=PROPERTY_DEFINITION('material property','material name',#13314);
#7973=PROPERTY_DEFINITION('material property','density of part',#13314);
#7974=PROPERTY_DEFINITION('material property','material name',#13315);
#7975=PROPERTY_DEFINITION('material property','density of part',#13315);
#7976=PROPERTY_DEFINITION('material property','material name',#13317);
#7977=PROPERTY_DEFINITION('material property','density of part',#13317);
#7978=PROPERTY_DEFINITION('material property','material name',#13318);
#7979=PROPERTY_DEFINITION('material property','density of part',#13318);
#7980=PROPERTY_DEFINITION('material property','material name',#13319);
#7981=PROPERTY_DEFINITION('material property','density of part',#13319);
#7982=PROPERTY_DEFINITION('material property','material name',#13320);
#7983=PROPERTY_DEFINITION('material property','density of part',#13320);
#7984=PROPERTY_DEFINITION('material property','material name',#13321);
#7985=PROPERTY_DEFINITION('material property','density of part',#13321);
#7986=AXIS2_PLACEMENT_3D('',#10899,#8698,#8699);
#7987=AXIS2_PLACEMENT_3D('',#10900,#8700,#8701);
#7988=AXIS2_PLACEMENT_3D('',#10901,#8702,#8703);
#7989=AXIS2_PLACEMENT_3D('',#10902,#8704,#8705);
#7990=AXIS2_PLACEMENT_3D('',#10904,#8706,#8707);
#7991=AXIS2_PLACEMENT_3D('',#10907,#8709,#8710);
#7992=AXIS2_PLACEMENT_3D('',#10908,#8711,#8712);
#7993=AXIS2_PLACEMENT_3D('',#10910,#8713,#8714);
#7994=AXIS2_PLACEMENT_3D('',#10913,#8716,#8717);
#7995=AXIS2_PLACEMENT_3D('',#10914,#8718,#8719);
#7996=AXIS2_PLACEMENT_3D('',#10916,#8720,#8721);
#7997=AXIS2_PLACEMENT_3D('',#10919,#8723,#8724);
#7998=AXIS2_PLACEMENT_3D('',#10920,#8725,#8726);
#7999=AXIS2_PLACEMENT_3D('',#10922,#8727,#8728);
#8000=AXIS2_PLACEMENT_3D('',#10925,#8730,#8731);
#8001=AXIS2_PLACEMENT_3D('',#10926,#8732,#8733);
#8002=AXIS2_PLACEMENT_3D('',#10935,#8738,#8739);
#8003=AXIS2_PLACEMENT_3D('',#10941,#8743,#8744);
#8004=AXIS2_PLACEMENT_3D('',#10947,#8748,#8749);
#8005=AXIS2_PLACEMENT_3D('',#10950,#8752,#8753);
#8006=AXIS2_PLACEMENT_3D('',#10951,#8754,#8755);
#8007=AXIS2_PLACEMENT_3D('',#10952,#8756,#8757);
#8008=AXIS2_PLACEMENT_3D('',#10953,#8758,#8759);
#8009=AXIS2_PLACEMENT_3D('',#10955,#8760,#8761);
#8010=AXIS2_PLACEMENT_3D('',#10958,#8763,#8764);
#8011=AXIS2_PLACEMENT_3D('',#10959,#8765,#8766);
#8012=AXIS2_PLACEMENT_3D('',#10961,#8767,#8768);
#8013=AXIS2_PLACEMENT_3D('',#10964,#8770,#8771);
#8014=AXIS2_PLACEMENT_3D('',#10965,#8772,#8773);
#8015=AXIS2_PLACEMENT_3D('',#10967,#8774,#8775);
#8016=AXIS2_PLACEMENT_3D('',#10970,#8777,#8778);
#8017=AXIS2_PLACEMENT_3D('',#10971,#8779,#8780);
#8018=AXIS2_PLACEMENT_3D('',#10973,#8781,#8782);
#8019=AXIS2_PLACEMENT_3D('',#10976,#8784,#8785);
#8020=AXIS2_PLACEMENT_3D('',#10977,#8786,#8787);
#8021=AXIS2_PLACEMENT_3D('',#10986,#8792,#8793);
#8022=AXIS2_PLACEMENT_3D('',#10992,#8797,#8798);
#8023=AXIS2_PLACEMENT_3D('',#10998,#8802,#8803);
#8024=AXIS2_PLACEMENT_3D('',#11001,#8806,#8807);
#8025=AXIS2_PLACEMENT_3D('',#11010,#8812,#8813);
#8026=AXIS2_PLACEMENT_3D('',#11016,#8817,#8818);
#8027=AXIS2_PLACEMENT_3D('',#11022,#8822,#8823);
#8028=AXIS2_PLACEMENT_3D('',#11025,#8826,#8827);
#8029=AXIS2_PLACEMENT_3D('',#11026,#8828,#8829);
#8030=AXIS2_PLACEMENT_3D('',#11027,#8830,#8831);
#8031=AXIS2_PLACEMENT_3D('',#11028,#8832,#8833);
#8032=AXIS2_PLACEMENT_3D('',#11037,#8838,#8839);
#8033=AXIS2_PLACEMENT_3D('',#11043,#8843,#8844);
#8034=AXIS2_PLACEMENT_3D('',#11049,#8848,#8849);
#8035=AXIS2_PLACEMENT_3D('',#11052,#8852,#8853);
#8036=AXIS2_PLACEMENT_3D('',#11053,#8854,#8855);
#8037=AXIS2_PLACEMENT_3D('',#11054,#8856,#8857);
#8038=AXIS2_PLACEMENT_3D('',#11055,#8858,#8859);
#8039=AXIS2_PLACEMENT_3D('',#11064,#8864,#8865);
#8040=AXIS2_PLACEMENT_3D('',#11070,#8869,#8870);
#8041=AXIS2_PLACEMENT_3D('',#11076,#8874,#8875);
#8042=AXIS2_PLACEMENT_3D('',#11079,#8878,#8879);
#8043=AXIS2_PLACEMENT_3D('',#11080,#8880,#8881);
#8044=AXIS2_PLACEMENT_3D('',#11081,#8882,#8883);
#8045=AXIS2_PLACEMENT_3D('',#11082,#8884,#8885);
#8046=AXIS2_PLACEMENT_3D('',#11091,#8890,#8891);
#8047=AXIS2_PLACEMENT_3D('',#11097,#8895,#8896);
#8048=AXIS2_PLACEMENT_3D('',#11103,#8900,#8901);
#8049=AXIS2_PLACEMENT_3D('',#11106,#8904,#8905);
#8050=AXIS2_PLACEMENT_3D('',#11107,#8906,#8907);
#8051=AXIS2_PLACEMENT_3D('',#11108,#8908,#8909);
#8052=AXIS2_PLACEMENT_3D('',#11109,#8910,#8911);
#8053=AXIS2_PLACEMENT_3D('',#11111,#8912,#8913);
#8054=AXIS2_PLACEMENT_3D('',#11114,#8915,#8916);
#8055=AXIS2_PLACEMENT_3D('',#11115,#8917,#8918);
#8056=AXIS2_PLACEMENT_3D('',#11117,#8919,#8920);
#8057=AXIS2_PLACEMENT_3D('',#11120,#8922,#8923);
#8058=AXIS2_PLACEMENT_3D('',#11121,#8924,#8925);
#8059=AXIS2_PLACEMENT_3D('',#11130,#8930,#8931);
#8060=AXIS2_PLACEMENT_3D('',#11136,#8935,#8936);
#8061=AXIS2_PLACEMENT_3D('',#11142,#8940,#8941);
#8062=AXIS2_PLACEMENT_3D('',#11145,#8944,#8945);
#8063=AXIS2_PLACEMENT_3D('',#11146,#8946,#8947);
#8064=AXIS2_PLACEMENT_3D('',#11147,#8948,#8949);
#8065=AXIS2_PLACEMENT_3D('',#11148,#8950,#8951);
#8066=AXIS2_PLACEMENT_3D('',#11150,#8952,#8953);
#8067=AXIS2_PLACEMENT_3D('',#11153,#8955,#8956);
#8068=AXIS2_PLACEMENT_3D('',#11154,#8957,#8958);
#8069=AXIS2_PLACEMENT_3D('',#11156,#8959,#8960);
#8070=AXIS2_PLACEMENT_3D('',#11159,#8962,#8963);
#8071=AXIS2_PLACEMENT_3D('',#11160,#8964,#8965);
#8072=AXIS2_PLACEMENT_3D('',#11169,#8970,#8971);
#8073=AXIS2_PLACEMENT_3D('',#11175,#8975,#8976);
#8074=AXIS2_PLACEMENT_3D('',#11181,#8980,#8981);
#8075=AXIS2_PLACEMENT_3D('',#11184,#8984,#8985);
#8076=AXIS2_PLACEMENT_3D('',#11185,#8986,#8987);
#8077=AXIS2_PLACEMENT_3D('',#11186,#8988,#8989);
#8078=AXIS2_PLACEMENT_3D('',#11187,#8990,#8991);
#8079=AXIS2_PLACEMENT_3D('',#11189,#8992,#8993);
#8080=AXIS2_PLACEMENT_3D('',#11192,#8995,#8996);
#8081=AXIS2_PLACEMENT_3D('',#11193,#8997,#8998);
#8082=AXIS2_PLACEMENT_3D('',#11194,#8999,#9000);
#8083=AXIS2_PLACEMENT_3D('',#11196,#9001,#9002);
#8084=AXIS2_PLACEMENT_3D('',#11199,#9004,#9005);
#8085=AXIS2_PLACEMENT_3D('',#11200,#9006,#9007);
#8086=AXIS2_PLACEMENT_3D('',#11202,#9008,#9009);
#8087=AXIS2_PLACEMENT_3D('',#11203,#9010,#9011);
#8088=AXIS2_PLACEMENT_3D('',#11205,#9012,#9013);
#8089=AXIS2_PLACEMENT_3D('',#11207,#9015,#9016);
#8090=AXIS2_PLACEMENT_3D('',#11216,#9021,#9022);
#8091=AXIS2_PLACEMENT_3D('',#11222,#9026,#9027);
#8092=AXIS2_PLACEMENT_3D('',#11228,#9031,#9032);
#8093=AXIS2_PLACEMENT_3D('',#11231,#9035,#9036);
#8094=AXIS2_PLACEMENT_3D('',#11232,#9037,#9038);
#8095=AXIS2_PLACEMENT_3D('',#11233,#9039,#9040);
#8096=AXIS2_PLACEMENT_3D('',#11234,#9041,#9042);
#8097=AXIS2_PLACEMENT_3D('',#11236,#9043,#9044);
#8098=AXIS2_PLACEMENT_3D('',#11239,#9046,#9047);
#8099=AXIS2_PLACEMENT_3D('',#11240,#9048,#9049);
#8100=AXIS2_PLACEMENT_3D('',#11241,#9050,#9051);
#8101=AXIS2_PLACEMENT_3D('',#11243,#9052,#9053);
#8102=AXIS2_PLACEMENT_3D('',#11246,#9055,#9056);
#8103=AXIS2_PLACEMENT_3D('',#11247,#9057,#9058);
#8104=AXIS2_PLACEMENT_3D('',#11249,#9059,#9060);
#8105=AXIS2_PLACEMENT_3D('',#11250,#9061,#9062);
#8106=AXIS2_PLACEMENT_3D('',#11253,#9064,#9065);
#8107=AXIS2_PLACEMENT_3D('',#11254,#9066,#9067);
#8108=AXIS2_PLACEMENT_3D('',#11263,#9072,#9073);
#8109=AXIS2_PLACEMENT_3D('',#11269,#9077,#9078);
#8110=AXIS2_PLACEMENT_3D('',#11275,#9082,#9083);
#8111=AXIS2_PLACEMENT_3D('',#11278,#9086,#9087);
#8112=AXIS2_PLACEMENT_3D('',#11279,#9088,#9089);
#8113=AXIS2_PLACEMENT_3D('',#11280,#9090,#9091);
#8114=AXIS2_PLACEMENT_3D('',#11281,#9092,#9093);
#8115=AXIS2_PLACEMENT_3D('',#11283,#9094,#9095);
#8116=AXIS2_PLACEMENT_3D('',#11286,#9097,#9098);
#8117=AXIS2_PLACEMENT_3D('',#11287,#9099,#9100);
#8118=AXIS2_PLACEMENT_3D('',#11288,#9101,#9102);
#8119=AXIS2_PLACEMENT_3D('',#11290,#9103,#9104);
#8120=AXIS2_PLACEMENT_3D('',#11293,#9106,#9107);
#8121=AXIS2_PLACEMENT_3D('',#11294,#9108,#9109);
#8122=AXIS2_PLACEMENT_3D('',#11296,#9110,#9111);
#8123=AXIS2_PLACEMENT_3D('',#11297,#9112,#9113);
#8124=AXIS2_PLACEMENT_3D('',#11299,#9114,#9115);
#8125=AXIS2_PLACEMENT_3D('',#11301,#9117,#9118);
#8126=AXIS2_PLACEMENT_3D('',#11310,#9123,#9124);
#8127=AXIS2_PLACEMENT_3D('',#11316,#9128,#9129);
#8128=AXIS2_PLACEMENT_3D('',#11322,#9133,#9134);
#8129=AXIS2_PLACEMENT_3D('',#11325,#9137,#9138);
#8130=AXIS2_PLACEMENT_3D('',#11326,#9139,#9140);
#8131=AXIS2_PLACEMENT_3D('',#11327,#9141,#9142);
#8132=AXIS2_PLACEMENT_3D('',#11328,#9143,#9144);
#8133=AXIS2_PLACEMENT_3D('',#11330,#9145,#9146);
#8134=AXIS2_PLACEMENT_3D('',#11333,#9148,#9149);
#8135=AXIS2_PLACEMENT_3D('',#11334,#9150,#9151);
#8136=AXIS2_PLACEMENT_3D('',#11335,#9152,#9153);
#8137=AXIS2_PLACEMENT_3D('',#11337,#9154,#9155);
#8138=AXIS2_PLACEMENT_3D('',#11340,#9157,#9158);
#8139=AXIS2_PLACEMENT_3D('',#11341,#9159,#9160);
#8140=AXIS2_PLACEMENT_3D('',#11343,#9161,#9162);
#8141=AXIS2_PLACEMENT_3D('',#11344,#9163,#9164);
#8142=AXIS2_PLACEMENT_3D('',#11347,#9166,#9167);
#8143=AXIS2_PLACEMENT_3D('',#11348,#9168,#9169);
#8144=AXIS2_PLACEMENT_3D('',#11357,#9174,#9175);
#8145=AXIS2_PLACEMENT_3D('',#11363,#9179,#9180);
#8146=AXIS2_PLACEMENT_3D('',#11369,#9184,#9185);
#8147=AXIS2_PLACEMENT_3D('',#11372,#9188,#9189);
#8148=AXIS2_PLACEMENT_3D('',#11373,#9190,#9191);
#8149=AXIS2_PLACEMENT_3D('',#11374,#9192,#9193);
#8150=AXIS2_PLACEMENT_3D('',#11375,#9194,#9195);
#8151=AXIS2_PLACEMENT_3D('',#11384,#9200,#9201);
#8152=AXIS2_PLACEMENT_3D('',#11390,#9205,#9206);
#8153=AXIS2_PLACEMENT_3D('',#11396,#9210,#9211);
#8154=AXIS2_PLACEMENT_3D('',#11399,#9214,#9215);
#8155=AXIS2_PLACEMENT_3D('',#11408,#9220,#9221);
#8156=AXIS2_PLACEMENT_3D('',#11414,#9225,#9226);
#8157=AXIS2_PLACEMENT_3D('',#11420,#9230,#9231);
#8158=AXIS2_PLACEMENT_3D('',#11423,#9234,#9235);
#8159=AXIS2_PLACEMENT_3D('',#11424,#9236,#9237);
#8160=AXIS2_PLACEMENT_3D('',#11425,#9238,#9239);
#8161=AXIS2_PLACEMENT_3D('',#11426,#9240,#9241);
#8162=AXIS2_PLACEMENT_3D('',#11435,#9246,#9247);
#8163=AXIS2_PLACEMENT_3D('',#11441,#9251,#9252);
#8164=AXIS2_PLACEMENT_3D('',#11447,#9256,#9257);
#8165=AXIS2_PLACEMENT_3D('',#11450,#9260,#9261);
#8166=AXIS2_PLACEMENT_3D('',#11459,#9266,#9267);
#8167=AXIS2_PLACEMENT_3D('',#11465,#9271,#9272);
#8168=AXIS2_PLACEMENT_3D('',#11471,#9276,#9277);
#8169=AXIS2_PLACEMENT_3D('',#11474,#9280,#9281);
#8170=AXIS2_PLACEMENT_3D('',#11475,#9282,#9283);
#8171=AXIS2_PLACEMENT_3D('',#11476,#9284,#9285);
#8172=AXIS2_PLACEMENT_3D('',#11477,#9286,#9287);
#8173=AXIS2_PLACEMENT_3D('',#11479,#9288,#9289);
#8174=AXIS2_PLACEMENT_3D('',#11482,#9291,#9292);
#8175=AXIS2_PLACEMENT_3D('',#11483,#9293,#9294);
#8176=AXIS2_PLACEMENT_3D('',#11485,#9295,#9296);
#8177=AXIS2_PLACEMENT_3D('',#11488,#9298,#9299);
#8178=AXIS2_PLACEMENT_3D('',#11489,#9300,#9301);
#8179=AXIS2_PLACEMENT_3D('',#11491,#9302,#9303);
#8180=AXIS2_PLACEMENT_3D('',#11494,#9305,#9306);
#8181=AXIS2_PLACEMENT_3D('',#11495,#9307,#9308);
#8182=AXIS2_PLACEMENT_3D('',#11497,#9309,#9310);
#8183=AXIS2_PLACEMENT_3D('',#11500,#9312,#9313);
#8184=AXIS2_PLACEMENT_3D('',#11501,#9314,#9315);
#8185=AXIS2_PLACEMENT_3D('',#11503,#9316,#9317);
#8186=AXIS2_PLACEMENT_3D('',#11506,#9319,#9320);
#8187=AXIS2_PLACEMENT_3D('',#11507,#9321,#9322);
#8188=AXIS2_PLACEMENT_3D('',#11509,#9323,#9324);
#8189=AXIS2_PLACEMENT_3D('',#11512,#9326,#9327);
#8190=AXIS2_PLACEMENT_3D('',#11513,#9328,#9329);
#8191=AXIS2_PLACEMENT_3D('',#11515,#9330,#9331);
#8192=AXIS2_PLACEMENT_3D('',#11518,#9333,#9334);
#8193=AXIS2_PLACEMENT_3D('',#11519,#9335,#9336);
#8194=AXIS2_PLACEMENT_3D('',#11521,#9337,#9338);
#8195=AXIS2_PLACEMENT_3D('',#11524,#9340,#9341);
#8196=AXIS2_PLACEMENT_3D('',#11525,#9342,#9343);
#8197=AXIS2_PLACEMENT_3D('',#11534,#9348,#9349);
#8198=AXIS2_PLACEMENT_3D('',#11540,#9353,#9354);
#8199=AXIS2_PLACEMENT_3D('',#11546,#9358,#9359);
#8200=AXIS2_PLACEMENT_3D('',#11549,#9362,#9363);
#8201=AXIS2_PLACEMENT_3D('',#11550,#9364,#9365);
#8202=AXIS2_PLACEMENT_3D('',#11551,#9366,#9367);
#8203=AXIS2_PLACEMENT_3D('',#11552,#9368,#9369);
#8204=AXIS2_PLACEMENT_3D('',#11554,#9370,#9371);
#8205=AXIS2_PLACEMENT_3D('',#11557,#9373,#9374);
#8206=AXIS2_PLACEMENT_3D('',#11558,#9375,#9376);
#8207=AXIS2_PLACEMENT_3D('',#11560,#9377,#9378);
#8208=AXIS2_PLACEMENT_3D('',#11563,#9380,#9381);
#8209=AXIS2_PLACEMENT_3D('',#11564,#9382,#9383);
#8210=AXIS2_PLACEMENT_3D('',#11573,#9388,#9389);
#8211=AXIS2_PLACEMENT_3D('',#11579,#9393,#9394);
#8212=AXIS2_PLACEMENT_3D('',#11585,#9398,#9399);
#8213=AXIS2_PLACEMENT_3D('',#11591,#9403,#9404);
#8214=AXIS2_PLACEMENT_3D('',#11597,#9408,#9409);
#8215=AXIS2_PLACEMENT_3D('',#11600,#9412,#9413);
#8216=AXIS2_PLACEMENT_3D('',#11601,#9414,#9415);
#8217=AXIS2_PLACEMENT_3D('',#11602,#9416,#9417);
#8218=AXIS2_PLACEMENT_3D('',#11603,#9418,#9419);
#8219=AXIS2_PLACEMENT_3D('',#11605,#9420,#9421);
#8220=AXIS2_PLACEMENT_3D('',#11608,#9423,#9424);
#8221=AXIS2_PLACEMENT_3D('',#11609,#9425,#9426);
#8222=AXIS2_PLACEMENT_3D('',#11610,#9427,#9428);
#8223=AXIS2_PLACEMENT_3D('',#11612,#9429,#9430);
#8224=AXIS2_PLACEMENT_3D('',#11615,#9432,#9433);
#8225=AXIS2_PLACEMENT_3D('',#11616,#9434,#9435);
#8226=AXIS2_PLACEMENT_3D('',#11625,#9440,#9441);
#8227=AXIS2_PLACEMENT_3D('',#11631,#9445,#9446);
#8228=AXIS2_PLACEMENT_3D('',#11635,#9449,#9450);
#8229=AXIS2_PLACEMENT_3D('',#11643,#9455,#9456);
#8230=AXIS2_PLACEMENT_3D('',#11649,#9460,#9461);
#8231=AXIS2_PLACEMENT_3D('',#11653,#9464,#9465);
#8232=AXIS2_PLACEMENT_3D('',#11657,#9468,#9469);
#8233=AXIS2_PLACEMENT_3D('',#11659,#9471,#9472);
#8234=AXIS2_PLACEMENT_3D('',#11660,#9473,#9474);
#8235=AXIS2_PLACEMENT_3D('',#11661,#9475,#9476);
#8236=AXIS2_PLACEMENT_3D('',#11663,#9477,#9478);
#8237=AXIS2_PLACEMENT_3D('',#11666,#9480,#9481);
#8238=AXIS2_PLACEMENT_3D('',#11667,#9482,#9483);
#8239=AXIS2_PLACEMENT_3D('',#11668,#9484,#9485);
#8240=AXIS2_PLACEMENT_3D('',#11670,#9486,#9487);
#8241=AXIS2_PLACEMENT_3D('',#11673,#9489,#9490);
#8242=AXIS2_PLACEMENT_3D('',#11674,#9491,#9492);
#8243=AXIS2_PLACEMENT_3D('',#11683,#9497,#9498);
#8244=AXIS2_PLACEMENT_3D('',#11689,#9502,#9503);
#8245=AXIS2_PLACEMENT_3D('',#11693,#9506,#9507);
#8246=AXIS2_PLACEMENT_3D('',#11701,#9512,#9513);
#8247=AXIS2_PLACEMENT_3D('',#11707,#9517,#9518);
#8248=AXIS2_PLACEMENT_3D('',#11711,#9521,#9522);
#8249=AXIS2_PLACEMENT_3D('',#11715,#9525,#9526);
#8250=AXIS2_PLACEMENT_3D('',#11717,#9528,#9529);
#8251=AXIS2_PLACEMENT_3D('',#11718,#9530,#9531);
#8252=AXIS2_PLACEMENT_3D('',#11719,#9532,#9533);
#8253=AXIS2_PLACEMENT_3D('',#11721,#9534,#9535);
#8254=AXIS2_PLACEMENT_3D('',#11724,#9537,#9538);
#8255=AXIS2_PLACEMENT_3D('',#11725,#9539,#9540);
#8256=AXIS2_PLACEMENT_3D('',#11734,#9545,#9546);
#8257=AXIS2_PLACEMENT_3D('',#11740,#9550,#9551);
#8258=AXIS2_PLACEMENT_3D('',#11746,#9555,#9556);
#8259=AXIS2_PLACEMENT_3D('',#11749,#9559,#9560);
#8260=AXIS2_PLACEMENT_3D('',#11750,#9561,#9562);
#8261=AXIS2_PLACEMENT_3D('',#11751,#9563,#9564);
#8262=AXIS2_PLACEMENT_3D('',#11752,#9565,#9566);
#8263=AXIS2_PLACEMENT_3D('',#11754,#9567,#9568);
#8264=AXIS2_PLACEMENT_3D('',#11757,#9570,#9571);
#8265=AXIS2_PLACEMENT_3D('',#11758,#9572,#9573);
#8266=AXIS2_PLACEMENT_3D('',#11767,#9578,#9579);
#8267=AXIS2_PLACEMENT_3D('',#11773,#9583,#9584);
#8268=AXIS2_PLACEMENT_3D('',#11779,#9588,#9589);
#8269=AXIS2_PLACEMENT_3D('',#11782,#9592,#9593);
#8270=AXIS2_PLACEMENT_3D('',#11783,#9594,#9595);
#8271=AXIS2_PLACEMENT_3D('',#11784,#9596,#9597);
#8272=AXIS2_PLACEMENT_3D('',#11785,#9598,#9599);
#8273=AXIS2_PLACEMENT_3D('',#11794,#9604,#9605);
#8274=AXIS2_PLACEMENT_3D('',#11800,#9609,#9610);
#8275=AXIS2_PLACEMENT_3D('',#11806,#9614,#9615);
#8276=AXIS2_PLACEMENT_3D('',#11812,#9619,#9620);
#8277=AXIS2_PLACEMENT_3D('',#11818,#9624,#9625);
#8278=AXIS2_PLACEMENT_3D('',#11824,#9629,#9630);
#8279=AXIS2_PLACEMENT_3D('',#11830,#9634,#9635);
#8280=AXIS2_PLACEMENT_3D('',#11836,#9639,#9640);
#8281=AXIS2_PLACEMENT_3D('',#11842,#9644,#9645);
#8282=AXIS2_PLACEMENT_3D('',#11851,#9650,#9651);
#8283=AXIS2_PLACEMENT_3D('',#11857,#9655,#9656);
#8284=AXIS2_PLACEMENT_3D('',#11863,#9660,#9661);
#8285=AXIS2_PLACEMENT_3D('',#11869,#9665,#9666);
#8286=AXIS2_PLACEMENT_3D('',#11875,#9670,#9671);
#8287=AXIS2_PLACEMENT_3D('',#11881,#9675,#9676);
#8288=AXIS2_PLACEMENT_3D('',#11887,#9680,#9681);
#8289=AXIS2_PLACEMENT_3D('',#11893,#9685,#9686);
#8290=AXIS2_PLACEMENT_3D('',#11899,#9690,#9691);
#8291=AXIS2_PLACEMENT_3D('',#11908,#9696,#9697);
#8292=AXIS2_PLACEMENT_3D('',#11914,#9701,#9702);
#8293=AXIS2_PLACEMENT_3D('',#11920,#9706,#9707);
#8294=AXIS2_PLACEMENT_3D('',#11926,#9711,#9712);
#8295=AXIS2_PLACEMENT_3D('',#11932,#9716,#9717);
#8296=AXIS2_PLACEMENT_3D('',#11938,#9721,#9722);
#8297=AXIS2_PLACEMENT_3D('',#11944,#9726,#9727);
#8298=AXIS2_PLACEMENT_3D('',#11950,#9731,#9732);
#8299=AXIS2_PLACEMENT_3D('',#11956,#9736,#9737);
#8300=AXIS2_PLACEMENT_3D('',#11965,#9742,#9743);
#8301=AXIS2_PLACEMENT_3D('',#11971,#9747,#9748);
#8302=AXIS2_PLACEMENT_3D('',#11977,#9752,#9753);
#8303=AXIS2_PLACEMENT_3D('',#11983,#9757,#9758);
#8304=AXIS2_PLACEMENT_3D('',#11989,#9762,#9763);
#8305=AXIS2_PLACEMENT_3D('',#11995,#9767,#9768);
#8306=AXIS2_PLACEMENT_3D('',#12001,#9772,#9773);
#8307=AXIS2_PLACEMENT_3D('',#12007,#9777,#9778);
#8308=AXIS2_PLACEMENT_3D('',#12013,#9782,#9783);
#8309=AXIS2_PLACEMENT_3D('',#12015,#9784,#9785);
#8310=AXIS2_PLACEMENT_3D('',#12018,#9787,#9788);
#8311=AXIS2_PLACEMENT_3D('',#12019,#9789,#9790);
#8312=AXIS2_PLACEMENT_3D('',#12025,#9794,#9795);
#8313=AXIS2_PLACEMENT_3D('',#12031,#9799,#9800);
#8314=AXIS2_PLACEMENT_3D('',#12034,#9803,#9804);
#8315=AXIS2_PLACEMENT_3D('',#12040,#9808,#9809);
#8316=AXIS2_PLACEMENT_3D('',#12043,#9812,#9813);
#8317=AXIS2_PLACEMENT_3D('',#12049,#9817,#9818);
#8318=AXIS2_PLACEMENT_3D('',#12052,#9821,#9822);
#8319=AXIS2_PLACEMENT_3D('',#12055,#9825,#9826);
#8320=AXIS2_PLACEMENT_3D('',#12056,#9827,#9828);
#8321=AXIS2_PLACEMENT_3D('',#12057,#9829,#9830);
#8322=AXIS2_PLACEMENT_3D('',#12058,#9831,#9832);
#8323=AXIS2_PLACEMENT_3D('',#12060,#9833,#9834);
#8324=AXIS2_PLACEMENT_3D('',#12061,#9835,#9836);
#8325=AXIS2_PLACEMENT_3D('',#12063,#9837,#9838);
#8326=AXIS2_PLACEMENT_3D('',#12065,#9840,#9841);
#8327=AXIS2_PLACEMENT_3D('',#12067,#9842,#9843);
#8328=AXIS2_PLACEMENT_3D('',#12069,#9845,#9846);
#8329=AXIS2_PLACEMENT_3D('',#12071,#9847,#9848);
#8330=AXIS2_PLACEMENT_3D('',#12073,#9850,#9851);
#8331=AXIS2_PLACEMENT_3D('',#12075,#9852,#9853);
#8332=AXIS2_PLACEMENT_3D('',#12076,#9854,#9855);
#8333=AXIS2_PLACEMENT_3D('',#12078,#9856,#9857);
#8334=AXIS2_PLACEMENT_3D('',#12080,#9859,#9860);
#8335=AXIS2_PLACEMENT_3D('',#12082,#9861,#9862);
#8336=AXIS2_PLACEMENT_3D('',#12084,#9864,#9865);
#8337=AXIS2_PLACEMENT_3D('',#12086,#9866,#9867);
#8338=AXIS2_PLACEMENT_3D('',#12088,#9869,#9870);
#8339=AXIS2_PLACEMENT_3D('',#12089,#9871,#9872);
#8340=AXIS2_PLACEMENT_3D('',#12098,#9877,#9878);
#8341=AXIS2_PLACEMENT_3D('',#12104,#9882,#9883);
#8342=AXIS2_PLACEMENT_3D('',#12110,#9887,#9888);
#8343=AXIS2_PLACEMENT_3D('',#12116,#9892,#9893);
#8344=AXIS2_PLACEMENT_3D('',#12122,#9897,#9898);
#8345=AXIS2_PLACEMENT_3D('',#12125,#9901,#9902);
#8346=AXIS2_PLACEMENT_3D('',#12126,#9903,#9904);
#8347=AXIS2_PLACEMENT_3D('',#12127,#9905,#9906);
#8348=AXIS2_PLACEMENT_3D('',#12128,#9907,#9908);
#8349=AXIS2_PLACEMENT_3D('',#12130,#9909,#9910);
#8350=AXIS2_PLACEMENT_3D('',#12133,#9912,#9913);
#8351=AXIS2_PLACEMENT_3D('',#12134,#9914,#9915);
#8352=AXIS2_PLACEMENT_3D('',#12136,#9916,#9917);
#8353=AXIS2_PLACEMENT_3D('',#12137,#9918,#9919);
#8354=AXIS2_PLACEMENT_3D('',#12139,#9920,#9921);
#8355=AXIS2_PLACEMENT_3D('',#12142,#9923,#9924);
#8356=AXIS2_PLACEMENT_3D('',#12143,#9925,#9926);
#8357=AXIS2_PLACEMENT_3D('',#12145,#9927,#9928);
#8358=AXIS2_PLACEMENT_3D('',#12146,#9929,#9930);
#8359=AXIS2_PLACEMENT_3D('',#12148,#9931,#9932);
#8360=AXIS2_PLACEMENT_3D('',#12151,#9934,#9935);
#8361=AXIS2_PLACEMENT_3D('',#12152,#9936,#9937);
#8362=AXIS2_PLACEMENT_3D('',#12154,#9938,#9939);
#8363=AXIS2_PLACEMENT_3D('',#12155,#9940,#9941);
#8364=AXIS2_PLACEMENT_3D('',#12157,#9942,#9943);
#8365=AXIS2_PLACEMENT_3D('',#12160,#9945,#9946);
#8366=AXIS2_PLACEMENT_3D('',#12161,#9947,#9948);
#8367=AXIS2_PLACEMENT_3D('',#12163,#9949,#9950);
#8368=AXIS2_PLACEMENT_3D('',#12164,#9951,#9952);
#8369=AXIS2_PLACEMENT_3D('',#12166,#9953,#9954);
#8370=AXIS2_PLACEMENT_3D('',#12168,#9956,#9957);
#8371=AXIS2_PLACEMENT_3D('',#12170,#9958,#9959);
#8372=AXIS2_PLACEMENT_3D('',#12172,#9961,#9962);
#8373=AXIS2_PLACEMENT_3D('',#12174,#9963,#9964);
#8374=AXIS2_PLACEMENT_3D('',#12176,#9966,#9967);
#8375=AXIS2_PLACEMENT_3D('',#12178,#9968,#9969);
#8376=AXIS2_PLACEMENT_3D('',#12180,#9971,#9972);
#8377=AXIS2_PLACEMENT_3D('',#12189,#9977,#9978);
#8378=AXIS2_PLACEMENT_3D('',#12195,#9982,#9983);
#8379=AXIS2_PLACEMENT_3D('',#12201,#9987,#9988);
#8380=AXIS2_PLACEMENT_3D('',#12207,#9992,#9993);
#8381=AXIS2_PLACEMENT_3D('',#12213,#9997,#9998);
#8382=AXIS2_PLACEMENT_3D('',#12219,#10002,#10003);
#8383=AXIS2_PLACEMENT_3D('',#12225,#10007,#10008);
#8384=AXIS2_PLACEMENT_3D('',#12231,#10012,#10013);
#8385=AXIS2_PLACEMENT_3D('',#12237,#10017,#10018);
#8386=AXIS2_PLACEMENT_3D('',#12243,#10022,#10023);
#8387=AXIS2_PLACEMENT_3D('',#12249,#10027,#10028);
#8388=AXIS2_PLACEMENT_3D('',#12252,#10031,#10032);
#8389=AXIS2_PLACEMENT_3D('',#12253,#10033,#10034);
#8390=AXIS2_PLACEMENT_3D('',#12254,#10035,#10036);
#8391=AXIS2_PLACEMENT_3D('',#12255,#10037,#10038);
#8392=AXIS2_PLACEMENT_3D('',#12264,#10043,#10044);
#8393=AXIS2_PLACEMENT_3D('',#12270,#10048,#10049);
#8394=AXIS2_PLACEMENT_3D('',#12277,#10053,#10054);
#8395=AXIS2_PLACEMENT_3D('',#12278,#10055,#10056);
#8396=AXIS2_PLACEMENT_3D('',#12292,#10064,#10065);
#8397=AXIS2_PLACEMENT_3D('',#12296,#10068,#10069);
#8398=AXIS2_PLACEMENT_3D('',#12300,#10072,#10073);
#8399=AXIS2_PLACEMENT_3D('',#12310,#10079,#10080);
#8400=AXIS2_PLACEMENT_3D('',#12312,#10082,#10083);
#8401=AXIS2_PLACEMENT_3D('',#12316,#10085,#10086);
#8402=AXIS2_PLACEMENT_3D('',#12318,#10088,#10089);
#8403=AXIS2_PLACEMENT_3D('',#12320,#10090,#10091);
#8404=AXIS2_PLACEMENT_3D('',#12323,#10093,#10094);
#8405=AXIS2_PLACEMENT_3D('',#12325,#10095,#10096);
#8406=AXIS2_PLACEMENT_3D('',#12326,#10097,#10098);
#8407=AXIS2_PLACEMENT_3D('',#12327,#10099,#10100);
#8408=AXIS2_PLACEMENT_3D('',#12329,#10102,#10103);
#8409=AXIS2_PLACEMENT_3D('',#12331,#10105,#10106);
#8410=AXIS2_PLACEMENT_3D('',#12333,#10108,#10109);
#8411=AXIS2_PLACEMENT_3D('',#12334,#10110,#10111);
#8412=AXIS2_PLACEMENT_3D('',#12335,#10112,#10113);
#8413=AXIS2_PLACEMENT_3D('',#12337,#10114,#10115);
#8414=AXIS2_PLACEMENT_3D('',#12340,#10117,#10118);
#8415=AXIS2_PLACEMENT_3D('',#12341,#10119,#10120);
#8416=AXIS2_PLACEMENT_3D('',#12344,#10122,#10123);
#8417=AXIS2_PLACEMENT_3D('',#12345,#10124,#10125);
#8418=AXIS2_PLACEMENT_3D('',#12347,#10126,#10127);
#8419=AXIS2_PLACEMENT_3D('',#12348,#10128,#10129);
#8420=AXIS2_PLACEMENT_3D('',#12351,#10131,#10132);
#8421=AXIS2_PLACEMENT_3D('',#12352,#10133,#10134);
#8422=AXIS2_PLACEMENT_3D('',#12353,#10135,#10136);
#8423=AXIS2_PLACEMENT_3D('',#12354,#10137,#10138);
#8424=AXIS2_PLACEMENT_3D('',#12363,#10143,#10144);
#8425=AXIS2_PLACEMENT_3D('',#12369,#10148,#10149);
#8426=AXIS2_PLACEMENT_3D('',#12375,#10153,#10154);
#8427=AXIS2_PLACEMENT_3D('',#12381,#10158,#10159);
#8428=AXIS2_PLACEMENT_3D('',#12387,#10163,#10164);
#8429=AXIS2_PLACEMENT_3D('',#12390,#10167,#10168);
#8430=AXIS2_PLACEMENT_3D('',#12391,#10169,#10170);
#8431=AXIS2_PLACEMENT_3D('',#12392,#10171,#10172);
#8432=AXIS2_PLACEMENT_3D('',#12394,#10173,#10174);
#8433=AXIS2_PLACEMENT_3D('',#12396,#10175,#10176);
#8434=AXIS2_PLACEMENT_3D('',#12397,#10177,#10178);
#8435=AXIS2_PLACEMENT_3D('',#12400,#10180,#10181);
#8436=AXIS2_PLACEMENT_3D('',#12401,#10182,#10183);
#8437=AXIS2_PLACEMENT_3D('',#12402,#10184,#10185);
#8438=AXIS2_PLACEMENT_3D('',#12404,#10186,#10187);
#8439=AXIS2_PLACEMENT_3D('',#12405,#10188,#10189);
#8440=AXIS2_PLACEMENT_3D('',#12407,#10190,#10191);
#8441=AXIS2_PLACEMENT_3D('',#12409,#10193,#10194);
#8442=AXIS2_PLACEMENT_3D('',#12411,#10195,#10196);
#8443=AXIS2_PLACEMENT_3D('',#12413,#10198,#10199);
#8444=AXIS2_PLACEMENT_3D('',#12415,#10200,#10201);
#8445=AXIS2_PLACEMENT_3D('',#12417,#10203,#10204);
#8446=AXIS2_PLACEMENT_3D('',#12419,#10205,#10206);
#8447=AXIS2_PLACEMENT_3D('',#12420,#10207,#10208);
#8448=AXIS2_PLACEMENT_3D('',#12422,#10209,#10210);
#8449=AXIS2_PLACEMENT_3D('',#12424,#10212,#10213);
#8450=AXIS2_PLACEMENT_3D('',#12426,#10215,#10216);
#8451=AXIS2_PLACEMENT_3D('',#12427,#10217,#10218);
#8452=AXIS2_PLACEMENT_3D('',#12428,#10219,#10220);
#8453=AXIS2_PLACEMENT_3D('',#12430,#10221,#10222);
#8454=AXIS2_PLACEMENT_3D('',#12433,#10224,#10225);
#8455=AXIS2_PLACEMENT_3D('',#12434,#10226,#10227);
#8456=AXIS2_PLACEMENT_3D('',#12436,#10228,#10229);
#8457=AXIS2_PLACEMENT_3D('',#12439,#10231,#10232);
#8458=AXIS2_PLACEMENT_3D('',#12440,#10233,#10234);
#8459=AXIS2_PLACEMENT_3D('',#12442,#10235,#10236);
#8460=AXIS2_PLACEMENT_3D('',#12445,#10238,#10239);
#8461=AXIS2_PLACEMENT_3D('',#12446,#10240,#10241);
#8462=AXIS2_PLACEMENT_3D('',#12448,#10242,#10243);
#8463=AXIS2_PLACEMENT_3D('',#12451,#10245,#10246);
#8464=AXIS2_PLACEMENT_3D('',#12452,#10247,#10248);
#8465=AXIS2_PLACEMENT_3D('',#12454,#10249,#10250);
#8466=AXIS2_PLACEMENT_3D('',#12457,#10252,#10253);
#8467=AXIS2_PLACEMENT_3D('',#12458,#10254,#10255);
#8468=AXIS2_PLACEMENT_3D('',#12460,#10256,#10257);
#8469=AXIS2_PLACEMENT_3D('',#12463,#10259,#10260);
#8470=AXIS2_PLACEMENT_3D('',#12464,#10261,#10262);
#8471=AXIS2_PLACEMENT_3D('',#12473,#10267,#10268);
#8472=AXIS2_PLACEMENT_3D('',#12482,#10273,#10274);
#8473=AXIS2_PLACEMENT_3D('',#12485,#10277,#10278);
#8474=AXIS2_PLACEMENT_3D('',#12495,#10284,#10285);
#8475=AXIS2_PLACEMENT_3D('',#12499,#10288,#10289);
#8476=AXIS2_PLACEMENT_3D('',#12505,#10293,#10294);
#8477=AXIS2_PLACEMENT_3D('',#12507,#10296,#10297);
#8478=AXIS2_PLACEMENT_3D('',#12511,#10300,#10301);
#8479=AXIS2_PLACEMENT_3D('',#12513,#10303,#10304);
#8480=AXIS2_PLACEMENT_3D('',#12514,#10305,#10306);
#8481=AXIS2_PLACEMENT_3D('',#12515,#10307,#10308);
#8482=AXIS2_PLACEMENT_3D('',#12517,#10309,#10310);
#8483=AXIS2_PLACEMENT_3D('',#12520,#10312,#10313);
#8484=AXIS2_PLACEMENT_3D('',#12521,#10314,#10315);
#8485=AXIS2_PLACEMENT_3D('',#12522,#10316,#10317);
#8486=AXIS2_PLACEMENT_3D('',#12524,#10318,#10319);
#8487=AXIS2_PLACEMENT_3D('',#12527,#10321,#10322);
#8488=AXIS2_PLACEMENT_3D('',#12528,#10323,#10324);
#8489=AXIS2_PLACEMENT_3D('',#12529,#10325,#10326);
#8490=AXIS2_PLACEMENT_3D('',#12531,#10327,#10328);
#8491=AXIS2_PLACEMENT_3D('',#12535,#10330,#10331);
#8492=AXIS2_PLACEMENT_3D('',#12536,#10332,#10333);
#8493=AXIS2_PLACEMENT_3D('',#12537,#10334,#10335);
#8494=AXIS2_PLACEMENT_3D('',#12538,#10336,#10337);
#8495=AXIS2_PLACEMENT_3D('',#12540,#10339,#10340);
#8496=AXIS2_PLACEMENT_3D('',#12542,#10341,#10342);
#8497=AXIS2_PLACEMENT_3D('',#12543,#10343,#10344);
#8498=AXIS2_PLACEMENT_3D('',#12544,#10345,#10346);
#8499=AXIS2_PLACEMENT_3D('',#12546,#10347,#10348);
#8500=AXIS2_PLACEMENT_3D('',#12550,#10350,#10351);
#8501=AXIS2_PLACEMENT_3D('',#12551,#10352,#10353);
#8502=AXIS2_PLACEMENT_3D('',#12552,#10354,#10355);
#8503=AXIS2_PLACEMENT_3D('',#12553,#10356,#10357);
#8504=AXIS2_PLACEMENT_3D('',#12555,#10359,#10360);
#8505=AXIS2_PLACEMENT_3D('',#12557,#10361,#10362);
#8506=AXIS2_PLACEMENT_3D('',#12558,#10363,#10364);
#8507=AXIS2_PLACEMENT_3D('',#12559,#10365,#10366);
#8508=AXIS2_PLACEMENT_3D('',#12561,#10368,#10369);
#8509=AXIS2_PLACEMENT_3D('',#12562,#10370,#10371);
#8510=AXIS2_PLACEMENT_3D('',#12563,#10372,#10373);
#8511=AXIS2_PLACEMENT_3D('',#12567,#10375,#10376);
#8512=AXIS2_PLACEMENT_3D('',#12568,#10377,#10378);
#8513=AXIS2_PLACEMENT_3D('',#12572,#10380,#10381);
#8514=AXIS2_PLACEMENT_3D('',#12575,#10383,#10384);
#8515=AXIS2_PLACEMENT_3D('',#12577,#10385,#10386);
#8516=AXIS2_PLACEMENT_3D('',#12579,#10388,#10389);
#8517=AXIS2_PLACEMENT_3D('',#12583,#10391,#10392);
#8518=AXIS2_PLACEMENT_3D('',#12584,#10393,#10394);
#8519=AXIS2_PLACEMENT_3D('',#12588,#10396,#10397);
#8520=AXIS2_PLACEMENT_3D('',#12591,#10399,#10400);
#8521=AXIS2_PLACEMENT_3D('',#12593,#10401,#10402);
#8522=AXIS2_PLACEMENT_3D('',#12595,#10404,#10405);
#8523=AXIS2_PLACEMENT_3D('',#12599,#10407,#10408);
#8524=AXIS2_PLACEMENT_3D('',#12600,#10409,#10410);
#8525=AXIS2_PLACEMENT_3D('',#12604,#10412,#10413);
#8526=AXIS2_PLACEMENT_3D('',#12607,#10415,#10416);
#8527=AXIS2_PLACEMENT_3D('',#12609,#10417,#10418);
#8528=AXIS2_PLACEMENT_3D('',#12611,#10420,#10421);
#8529=AXIS2_PLACEMENT_3D('',#12615,#10423,#10424);
#8530=AXIS2_PLACEMENT_3D('',#12616,#10425,#10426);
#8531=AXIS2_PLACEMENT_3D('',#12620,#10428,#10429);
#8532=AXIS2_PLACEMENT_3D('',#12623,#10431,#10432);
#8533=AXIS2_PLACEMENT_3D('',#12625,#10433,#10434);
#8534=AXIS2_PLACEMENT_3D('',#12627,#10436,#10437);
#8535=AXIS2_PLACEMENT_3D('',#12638,#10444,#10445);
#8536=AXIS2_PLACEMENT_3D('',#12649,#10452,#10453);
#8537=AXIS2_PLACEMENT_3D('',#12668,#10464,#10465);
#8538=AXIS2_PLACEMENT_3D('',#12672,#10468,#10469);
#8539=AXIS2_PLACEMENT_3D('',#12676,#10472,#10473);
#8540=AXIS2_PLACEMENT_3D('',#12680,#10476,#10477);
#8541=AXIS2_PLACEMENT_3D('',#12684,#10480,#10481);
#8542=AXIS2_PLACEMENT_3D('',#12686,#10483,#10484);
#8543=AXIS2_PLACEMENT_3D('',#12690,#10487,#10488);
#8544=AXIS2_PLACEMENT_3D('',#12694,#10491,#10492);
#8545=AXIS2_PLACEMENT_3D('',#12698,#10495,#10496);
#8546=AXIS2_PLACEMENT_3D('',#12702,#10499,#10500);
#8547=AXIS2_PLACEMENT_3D('',#12704,#10502,#10503);
#8548=AXIS2_PLACEMENT_3D('',#12705,#10504,#10505);
#8549=AXIS2_PLACEMENT_3D('',#12706,#10506,#10507);
#8550=AXIS2_PLACEMENT_3D('',#12715,#10512,#10513);
#8551=AXIS2_PLACEMENT_3D('',#12721,#10517,#10518);
#8552=AXIS2_PLACEMENT_3D('',#12727,#10522,#10523);
#8553=AXIS2_PLACEMENT_3D('',#12733,#10527,#10528);
#8554=AXIS2_PLACEMENT_3D('',#12739,#10532,#10533);
#8555=AXIS2_PLACEMENT_3D('',#12745,#10537,#10538);
#8556=AXIS2_PLACEMENT_3D('',#12751,#10542,#10543);
#8557=AXIS2_PLACEMENT_3D('',#12754,#10546,#10547);
#8558=AXIS2_PLACEMENT_3D('',#12755,#10548,#10549);
#8559=AXIS2_PLACEMENT_3D('',#12756,#10550,#10551);
#8560=AXIS2_PLACEMENT_3D('',#12757,#10552,#10553);
#8561=AXIS2_PLACEMENT_3D('',#12766,#10558,#10559);
#8562=AXIS2_PLACEMENT_3D('',#12772,#10563,#10564);
#8563=AXIS2_PLACEMENT_3D('',#12778,#10568,#10569);
#8564=AXIS2_PLACEMENT_3D('',#12784,#10573,#10574);
#8565=AXIS2_PLACEMENT_3D('',#12790,#10578,#10579);
#8566=AXIS2_PLACEMENT_3D('',#12796,#10583,#10584);
#8567=AXIS2_PLACEMENT_3D('',#12802,#10588,#10589);
#8568=AXIS2_PLACEMENT_3D('',#12805,#10592,#10593);
#8569=AXIS2_PLACEMENT_3D('',#12806,#10594,#10595);
#8570=AXIS2_PLACEMENT_3D('',#12807,#10596,#10597);
#8571=AXIS2_PLACEMENT_3D('',#12808,#10598,#10599);
#8572=AXIS2_PLACEMENT_3D('',#12809,#10600,#10601);
#8573=AXIS2_PLACEMENT_3D('',#12810,#10602,#10603);
#8574=AXIS2_PLACEMENT_3D('',#12811,#10604,#10605);
#8575=AXIS2_PLACEMENT_3D('',#12820,#10610,#10611);
#8576=AXIS2_PLACEMENT_3D('',#12826,#10615,#10616);
#8577=AXIS2_PLACEMENT_3D('',#12832,#10620,#10621);
#8578=AXIS2_PLACEMENT_3D('',#12838,#10625,#10626);
#8579=AXIS2_PLACEMENT_3D('',#12844,#10630,#10631);
#8580=AXIS2_PLACEMENT_3D('',#12847,#10634,#10635);
#8581=AXIS2_PLACEMENT_3D('',#12848,#10636,#10637);
#8582=AXIS2_PLACEMENT_3D('',#12849,#10638,#10639);
#8583=AXIS2_PLACEMENT_3D('',#12851,#10640,#10641);
#8584=AXIS2_PLACEMENT_3D('',#12852,#10642,#10643);
#8585=AXIS2_PLACEMENT_3D('',#12854,#10644,#10645);
#8586=AXIS2_PLACEMENT_3D('',#12855,#10646,#10647);
#8587=AXIS2_PLACEMENT_3D('',#12857,#10648,#10649);
#8588=AXIS2_PLACEMENT_3D('',#12859,#10651,#10652);
#8589=AXIS2_PLACEMENT_3D('',#12861,#10653,#10654);
#8590=AXIS2_PLACEMENT_3D('',#12863,#10656,#10657);
#8591=AXIS2_PLACEMENT_3D('',#12865,#10658,#10659);
#8592=AXIS2_PLACEMENT_3D('',#12867,#10661,#10662);
#8593=AXIS2_PLACEMENT_3D('',#12869,#10663,#10664);
#8594=AXIS2_PLACEMENT_3D('',#12870,#10665,#10666);
#8595=AXIS2_PLACEMENT_3D('',#12872,#10667,#10668);
#8596=AXIS2_PLACEMENT_3D('',#12874,#10670,#10671);
#8597=AXIS2_PLACEMENT_3D('',#12876,#10673,#10674);
#8598=AXIS2_PLACEMENT_3D('',#12877,#10675,#10676);
#8599=AXIS2_PLACEMENT_3D('',#12879,#10677,#10678);
#8600=AXIS2_PLACEMENT_3D('',#12880,#10679,#10680);
#8601=AXIS2_PLACEMENT_3D('',#12882,#10681,#10682);
#8602=AXIS2_PLACEMENT_3D('',#12884,#10684,#10685);
#8603=AXIS2_PLACEMENT_3D('',#12886,#10686,#10687);
#8604=AXIS2_PLACEMENT_3D('',#12888,#10689,#10690);
#8605=AXIS2_PLACEMENT_3D('',#12890,#10691,#10692);
#8606=AXIS2_PLACEMENT_3D('',#12892,#10694,#10695);
#8607=AXIS2_PLACEMENT_3D('',#12894,#10696,#10697);
#8608=AXIS2_PLACEMENT_3D('',#12895,#10698,#10699);
#8609=AXIS2_PLACEMENT_3D('',#12897,#10700,#10701);
#8610=AXIS2_PLACEMENT_3D('',#12899,#10703,#10704);
#8611=AXIS2_PLACEMENT_3D('',#12901,#10705,#10706);
#8612=AXIS2_PLACEMENT_3D('',#12903,#10708,#10709);
#8613=AXIS2_PLACEMENT_3D('',#12905,#10710,#10711);
#8614=AXIS2_PLACEMENT_3D('',#12907,#10713,#10714);
#8615=AXIS2_PLACEMENT_3D('',#12908,#10715,#10716);
#8616=AXIS2_PLACEMENT_3D('',#12917,#10721,#10722);
#8617=AXIS2_PLACEMENT_3D('',#12923,#10726,#10727);
#8618=AXIS2_PLACEMENT_3D('',#12929,#10731,#10732);
#8619=AXIS2_PLACEMENT_3D('',#12935,#10736,#10737);
#8620=AXIS2_PLACEMENT_3D('',#12941,#10741,#10742);
#8621=AXIS2_PLACEMENT_3D('',#12944,#10745,#10746);
#8622=AXIS2_PLACEMENT_3D('',#12945,#10747,#10748);
#8623=AXIS2_PLACEMENT_3D('',#12946,#10749,#10750);
#8624=AXIS2_PLACEMENT_3D('',#12947,#10751,#10752);
#8625=AXIS2_PLACEMENT_3D('',#12948,#10753,#10754);
#8626=AXIS2_PLACEMENT_3D('',#12949,#10755,#10756);
#8627=AXIS2_PLACEMENT_3D('',#12950,#10757,#10758);
#8628=AXIS2_PLACEMENT_3D('',#12951,#10759,#10760);
#8629=AXIS2_PLACEMENT_3D('',#12952,#10761,#10762);
#8630=AXIS2_PLACEMENT_3D('',#12953,#10763,#10764);
#8631=AXIS2_PLACEMENT_3D('',#12954,#10765,#10766);
#8632=AXIS2_PLACEMENT_3D('',#12955,#10767,#10768);
#8633=AXIS2_PLACEMENT_3D('',#12956,#10769,#10770);
#8634=AXIS2_PLACEMENT_3D('',#12957,#10771,#10772);
#8635=AXIS2_PLACEMENT_3D('',#12958,#10773,#10774);
#8636=AXIS2_PLACEMENT_3D('',#12959,#10775,#10776);
#8637=AXIS2_PLACEMENT_3D('',#12960,#10777,#10778);
#8638=AXIS2_PLACEMENT_3D('',#12961,#10779,#10780);
#8639=AXIS2_PLACEMENT_3D('',#12962,#10781,#10782);
#8640=AXIS2_PLACEMENT_3D('',#12963,#10783,#10784);
#8641=AXIS2_PLACEMENT_3D('',#12964,#10785,#10786);
#8642=AXIS2_PLACEMENT_3D('',#12965,#10787,#10788);
#8643=AXIS2_PLACEMENT_3D('',#12966,#10789,#10790);
#8644=AXIS2_PLACEMENT_3D('',#12967,#10791,#10792);
#8645=AXIS2_PLACEMENT_3D('',#12968,#10793,#10794);
#8646=AXIS2_PLACEMENT_3D('',#12969,#10795,#10796);
#8647=AXIS2_PLACEMENT_3D('',#12970,#10797,#10798);
#8648=AXIS2_PLACEMENT_3D('',#12971,#10799,#10800);
#8649=AXIS2_PLACEMENT_3D('',#12972,#10801,#10802);
#8650=AXIS2_PLACEMENT_3D('',#12973,#10803,#10804);
#8651=AXIS2_PLACEMENT_3D('',#12974,#10805,#10806);
#8652=AXIS2_PLACEMENT_3D('',#12975,#10807,#10808);
#8653=AXIS2_PLACEMENT_3D('',#12976,#10809,#10810);
#8654=AXIS2_PLACEMENT_3D('',#12977,#10811,#10812);
#8655=AXIS2_PLACEMENT_3D('',#12978,#10813,#10814);
#8656=AXIS2_PLACEMENT_3D('',#12979,#10815,#10816);
#8657=AXIS2_PLACEMENT_3D('',#12980,#10817,#10818);
#8658=AXIS2_PLACEMENT_3D('',#12981,#10819,#10820);
#8659=AXIS2_PLACEMENT_3D('',#12982,#10821,#10822);
#8660=AXIS2_PLACEMENT_3D('',#12983,#10823,#10824);
#8661=AXIS2_PLACEMENT_3D('',#12984,#10825,#10826);
#8662=AXIS2_PLACEMENT_3D('',#12985,#10827,#10828);
#8663=AXIS2_PLACEMENT_3D('',#12986,#10829,#10830);
#8664=AXIS2_PLACEMENT_3D('',#12987,#10831,#10832);
#8665=AXIS2_PLACEMENT_3D('',#12988,#10833,#10834);
#8666=AXIS2_PLACEMENT_3D('',#12989,#10835,#10836);
#8667=AXIS2_PLACEMENT_3D('',#12990,#10837,#10838);
#8668=AXIS2_PLACEMENT_3D('',#12991,#10839,#10840);
#8669=AXIS2_PLACEMENT_3D('',#12992,#10841,#10842);
#8670=AXIS2_PLACEMENT_3D('',#12993,#10843,#10844);
#8671=AXIS2_PLACEMENT_3D('',#12994,#10845,#10846);
#8672=AXIS2_PLACEMENT_3D('',#12995,#10847,#10848);
#8673=AXIS2_PLACEMENT_3D('',#12996,#10849,#10850);
#8674=AXIS2_PLACEMENT_3D('',#12997,#10851,#10852);
#8675=AXIS2_PLACEMENT_3D('',#12998,#10853,#10854);
#8676=AXIS2_PLACEMENT_3D('',#12999,#10855,#10856);
#8677=AXIS2_PLACEMENT_3D('',#13000,#10857,#10858);
#8678=AXIS2_PLACEMENT_3D('',#13001,#10859,#10860);
#8679=AXIS2_PLACEMENT_3D('',#13002,#10861,#10862);
#8680=AXIS2_PLACEMENT_3D('',#13003,#10863,#10864);
#8681=AXIS2_PLACEMENT_3D('',#13004,#10865,#10866);
#8682=AXIS2_PLACEMENT_3D('',#13005,#10867,#10868);
#8683=AXIS2_PLACEMENT_3D('',#13006,#10869,#10870);
#8684=AXIS2_PLACEMENT_3D('',#13007,#10871,#10872);
#8685=AXIS2_PLACEMENT_3D('',#13008,#10873,#10874);
#8686=AXIS2_PLACEMENT_3D('',#13009,#10875,#10876);
#8687=AXIS2_PLACEMENT_3D('',#13010,#10877,#10878);
#8688=AXIS2_PLACEMENT_3D('',#13011,#10879,#10880);
#8689=AXIS2_PLACEMENT_3D('',#13012,#10881,#10882);
#8690=AXIS2_PLACEMENT_3D('',#13013,#10883,#10884);
#8691=AXIS2_PLACEMENT_3D('',#13014,#10885,#10886);
#8692=AXIS2_PLACEMENT_3D('',#13015,#10887,#10888);
#8693=AXIS2_PLACEMENT_3D('',#13016,#10889,#10890);
#8694=AXIS2_PLACEMENT_3D('',#13017,#10891,#10892);
#8695=AXIS2_PLACEMENT_3D('',#13018,#10893,#10894);
#8696=AXIS2_PLACEMENT_3D('',#13019,#10895,#10896);
#8697=AXIS2_PLACEMENT_3D('',#13020,#10897,#10898);
#8698=DIRECTION('axis',(0.,0.,1.));
#8699=DIRECTION('refdir',(1.,0.,0.));
#8700=DIRECTION('axis',(0.,0.,1.));
#8701=DIRECTION('refdir',(1.,0.,0.));
#8702=DIRECTION('axis',(0.,0.,1.));
#8703=DIRECTION('refdir',(1.,0.,0.));
#8704=DIRECTION('center_axis',(0.,0.,1.));
#8705=DIRECTION('ref_axis',(1.,0.,0.));
#8706=DIRECTION('center_axis',(0.,0.,1.));
#8707=DIRECTION('ref_axis',(1.,0.,0.));
#8708=DIRECTION('',(0.,0.,1.));
#8709=DIRECTION('center_axis',(0.,0.,-1.));
#8710=DIRECTION('ref_axis',(1.,0.,0.));
#8711=DIRECTION('center_axis',(0.,0.,1.));
#8712=DIRECTION('ref_axis',(1.,0.,0.));
#8713=DIRECTION('center_axis',(0.,0.,1.));
#8714=DIRECTION('ref_axis',(1.,0.,0.));
#8715=DIRECTION('',(0.,0.,1.));
#8716=DIRECTION('center_axis',(0.,0.,-1.));
#8717=DIRECTION('ref_axis',(1.,0.,0.));
#8718=DIRECTION('center_axis',(0.,0.,1.));
#8719=DIRECTION('ref_axis',(1.,0.,0.));
#8720=DIRECTION('center_axis',(0.,0.,1.));
#8721=DIRECTION('ref_axis',(1.,0.,0.));
#8722=DIRECTION('',(0.,0.,1.));
#8723=DIRECTION('center_axis',(0.,0.,-1.));
#8724=DIRECTION('ref_axis',(1.,0.,0.));
#8725=DIRECTION('center_axis',(0.,0.,1.));
#8726=DIRECTION('ref_axis',(1.,0.,0.));
#8727=DIRECTION('center_axis',(0.,0.,1.));
#8728=DIRECTION('ref_axis',(1.,0.,0.));
#8729=DIRECTION('',(0.,0.,1.));
#8730=DIRECTION('center_axis',(0.,0.,-1.));
#8731=DIRECTION('ref_axis',(1.,0.,0.));
#8732=DIRECTION('center_axis',(0.,1.,0.));
#8733=DIRECTION('ref_axis',(-1.,0.,0.));
#8734=DIRECTION('',(-1.,0.,0.));
#8735=DIRECTION('',(0.,0.,1.));
#8736=DIRECTION('',(-1.,0.,0.));
#8737=DIRECTION('',(0.,0.,1.));
#8738=DIRECTION('center_axis',(1.,0.,0.));
#8739=DIRECTION('ref_axis',(0.,1.,0.));
#8740=DIRECTION('',(0.,1.,0.));
#8741=DIRECTION('',(0.,1.,0.));
#8742=DIRECTION('',(0.,0.,1.));
#8743=DIRECTION('center_axis',(0.,-1.,0.));
#8744=DIRECTION('ref_axis',(1.,0.,0.));
#8745=DIRECTION('',(1.,0.,0.));
#8746=DIRECTION('',(1.,0.,0.));
#8747=DIRECTION('',(0.,0.,1.));
#8748=DIRECTION('center_axis',(-1.,0.,0.));
#8749=DIRECTION('ref_axis',(0.,-1.,0.));
#8750=DIRECTION('',(0.,-1.,0.));
#8751=DIRECTION('',(0.,-1.,0.));
#8752=DIRECTION('center_axis',(0.,0.,1.));
#8753=DIRECTION('ref_axis',(1.,0.,0.));
#8754=DIRECTION('center_axis',(0.,0.,1.));
#8755=DIRECTION('ref_axis',(1.,0.,0.));
#8756=DIRECTION('axis',(0.,0.,1.));
#8757=DIRECTION('refdir',(1.,0.,0.));
#8758=DIRECTION('center_axis',(0.,0.,1.));
#8759=DIRECTION('ref_axis',(1.,0.,0.));
#8760=DIRECTION('center_axis',(0.,0.,1.));
#8761=DIRECTION('ref_axis',(1.,0.,0.));
#8762=DIRECTION('',(0.,0.,1.));
#8763=DIRECTION('center_axis',(0.,0.,-1.));
#8764=DIRECTION('ref_axis',(1.,0.,0.));
#8765=DIRECTION('center_axis',(0.,0.,1.));
#8766=DIRECTION('ref_axis',(1.,0.,0.));
#8767=DIRECTION('center_axis',(0.,0.,1.));
#8768=DIRECTION('ref_axis',(1.,0.,0.));
#8769=DIRECTION('',(0.,0.,1.));
#8770=DIRECTION('center_axis',(0.,0.,-1.));
#8771=DIRECTION('ref_axis',(1.,0.,0.));
#8772=DIRECTION('center_axis',(0.,0.,1.));
#8773=DIRECTION('ref_axis',(1.,0.,0.));
#8774=DIRECTION('center_axis',(0.,0.,1.));
#8775=DIRECTION('ref_axis',(1.,0.,0.));
#8776=DIRECTION('',(0.,0.,1.));
#8777=DIRECTION('center_axis',(0.,0.,-1.));
#8778=DIRECTION('ref_axis',(1.,0.,0.));
#8779=DIRECTION('center_axis',(0.,0.,1.));
#8780=DIRECTION('ref_axis',(1.,0.,0.));
#8781=DIRECTION('center_axis',(0.,0.,1.));
#8782=DIRECTION('ref_axis',(1.,0.,0.));
#8783=DIRECTION('',(0.,0.,1.));
#8784=DIRECTION('center_axis',(0.,0.,-1.));
#8785=DIRECTION('ref_axis',(1.,0.,0.));
#8786=DIRECTION('center_axis',(0.,-1.,0.));
#8787=DIRECTION('ref_axis',(1.,0.,0.));
#8788=DIRECTION('',(-1.,0.,0.));
#8789=DIRECTION('',(0.,0.,1.));
#8790=DIRECTION('',(1.,0.,0.));
#8791=DIRECTION('',(0.,0.,1.));
#8792=DIRECTION('center_axis',(-1.,0.,0.));
#8793=DIRECTION('ref_axis',(0.,-1.,0.));
#8794=DIRECTION('',(0.,1.,0.));
#8795=DIRECTION('',(0.,-1.,0.));
#8796=DIRECTION('',(0.,0.,1.));
#8797=DIRECTION('center_axis',(0.,1.,0.));
#8798=DIRECTION('ref_axis',(-1.,0.,0.));
#8799=DIRECTION('',(1.,0.,0.));
#8800=DIRECTION('',(-1.,0.,0.));
#8801=DIRECTION('',(0.,0.,1.));
#8802=DIRECTION('center_axis',(1.,0.,0.));
#8803=DIRECTION('ref_axis',(0.,1.,0.));
#8804=DIRECTION('',(0.,-1.,0.));
#8805=DIRECTION('',(0.,1.,0.));
#8806=DIRECTION('center_axis',(0.,1.,0.));
#8807=DIRECTION('ref_axis',(-1.,0.,0.));
#8808=DIRECTION('',(-1.,0.,0.));
#8809=DIRECTION('',(0.,0.,1.));
#8810=DIRECTION('',(-1.,0.,0.));
#8811=DIRECTION('',(0.,0.,1.));
#8812=DIRECTION('center_axis',(1.,0.,0.));
#8813=DIRECTION('ref_axis',(0.,1.,0.));
#8814=DIRECTION('',(0.,1.,0.));
#8815=DIRECTION('',(0.,1.,0.));
#8816=DIRECTION('',(0.,0.,1.));
#8817=DIRECTION('center_axis',(0.,-1.,0.));
#8818=DIRECTION('ref_axis',(1.,0.,0.));
#8819=DIRECTION('',(1.,0.,0.));
#8820=DIRECTION('',(1.,0.,0.));
#8821=DIRECTION('',(0.,0.,1.));
#8822=DIRECTION('center_axis',(-1.,0.,0.));
#8823=DIRECTION('ref_axis',(0.,-1.,0.));
#8824=DIRECTION('',(0.,-1.,0.));
#8825=DIRECTION('',(0.,-1.,0.));
#8826=DIRECTION('center_axis',(0.,0.,1.));
#8827=DIRECTION('ref_axis',(1.,0.,0.));
#8828=DIRECTION('center_axis',(0.,0.,1.));
#8829=DIRECTION('ref_axis',(1.,0.,0.));
#8830=DIRECTION('axis',(0.,0.,1.));
#8831=DIRECTION('refdir',(1.,0.,0.));
#8832=DIRECTION('center_axis',(0.,1.,0.));
#8833=DIRECTION('ref_axis',(-1.,0.,0.));
#8834=DIRECTION('',(-1.,0.,0.));
#8835=DIRECTION('',(0.,0.,1.));
#8836=DIRECTION('',(-1.,0.,0.));
#8837=DIRECTION('',(0.,0.,1.));
#8838=DIRECTION('center_axis',(1.,0.,0.));
#8839=DIRECTION('ref_axis',(0.,1.,0.));
#8840=DIRECTION('',(0.,1.,0.));
#8841=DIRECTION('',(0.,1.,0.));
#8842=DIRECTION('',(0.,0.,1.));
#8843=DIRECTION('center_axis',(0.,-1.,0.));
#8844=DIRECTION('ref_axis',(1.,0.,0.));
#8845=DIRECTION('',(1.,0.,0.));
#8846=DIRECTION('',(1.,0.,0.));
#8847=DIRECTION('',(0.,0.,1.));
#8848=DIRECTION('center_axis',(-1.,0.,0.));
#8849=DIRECTION('ref_axis',(0.,-1.,0.));
#8850=DIRECTION('',(0.,-1.,0.));
#8851=DIRECTION('',(0.,-1.,0.));
#8852=DIRECTION('center_axis',(0.,0.,1.));
#8853=DIRECTION('ref_axis',(1.,0.,0.));
#8854=DIRECTION('center_axis',(0.,0.,1.));
#8855=DIRECTION('ref_axis',(1.,0.,0.));
#8856=DIRECTION('axis',(0.,0.,1.));
#8857=DIRECTION('refdir',(1.,0.,0.));
#8858=DIRECTION('center_axis',(0.,1.,0.));
#8859=DIRECTION('ref_axis',(-1.,0.,0.));
#8860=DIRECTION('',(-1.,0.,0.));
#8861=DIRECTION('',(0.,0.,1.));
#8862=DIRECTION('',(-1.,0.,0.));
#8863=DIRECTION('',(0.,0.,1.));
#8864=DIRECTION('center_axis',(1.,0.,0.));
#8865=DIRECTION('ref_axis',(0.,1.,0.));
#8866=DIRECTION('',(0.,1.,0.));
#8867=DIRECTION('',(0.,1.,0.));
#8868=DIRECTION('',(0.,0.,1.));
#8869=DIRECTION('center_axis',(0.,-1.,0.));
#8870=DIRECTION('ref_axis',(1.,0.,0.));
#8871=DIRECTION('',(1.,0.,0.));
#8872=DIRECTION('',(1.,0.,0.));
#8873=DIRECTION('',(0.,0.,1.));
#8874=DIRECTION('center_axis',(-1.,0.,0.));
#8875=DIRECTION('ref_axis',(0.,-1.,0.));
#8876=DIRECTION('',(0.,-1.,0.));
#8877=DIRECTION('',(0.,-1.,0.));
#8878=DIRECTION('center_axis',(0.,0.,1.));
#8879=DIRECTION('ref_axis',(1.,0.,0.));
#8880=DIRECTION('center_axis',(0.,0.,1.));
#8881=DIRECTION('ref_axis',(1.,0.,0.));
#8882=DIRECTION('axis',(0.,0.,1.));
#8883=DIRECTION('refdir',(1.,0.,0.));
#8884=DIRECTION('center_axis',(-1.,0.,0.));
#8885=DIRECTION('ref_axis',(0.,0.,1.));
#8886=DIRECTION('',(0.,0.,-1.));
#8887=DIRECTION('',(0.,1.,0.));
#8888=DIRECTION('',(0.,0.,1.));
#8889=DIRECTION('',(0.,1.,0.));
#8890=DIRECTION('center_axis',(0.233372952475324,0.,-0.972387301980517));
#8891=DIRECTION('ref_axis',(-0.972387301980517,0.,-0.233372952475324));
#8892=DIRECTION('',(0.972387301980517,0.,0.233372952475324));
#8893=DIRECTION('',(-0.972387301980517,0.,-0.233372952475324));
#8894=DIRECTION('',(0.,1.,0.));
#8895=DIRECTION('center_axis',(1.,0.,0.));
#8896=DIRECTION('ref_axis',(0.,0.,-1.));
#8897=DIRECTION('',(0.,0.,1.));
#8898=DIRECTION('',(0.,0.,-1.));
#8899=DIRECTION('',(0.,1.,0.));
#8900=DIRECTION('center_axis',(-0.233372952475324,0.,0.972387301980517));
#8901=DIRECTION('ref_axis',(0.972387301980517,0.,0.233372952475324));
#8902=DIRECTION('',(-0.972387301980517,0.,-0.233372952475324));
#8903=DIRECTION('',(0.972387301980517,0.,0.233372952475324));
#8904=DIRECTION('center_axis',(0.,1.,0.));
#8905=DIRECTION('ref_axis',(0.,0.,1.));
#8906=DIRECTION('center_axis',(0.,1.,0.));
#8907=DIRECTION('ref_axis',(1.,0.,0.));
#8908=DIRECTION('axis',(0.,0.,1.));
#8909=DIRECTION('refdir',(1.,0.,0.));
#8910=DIRECTION('center_axis',(0.,1.,0.));
#8911=DIRECTION('ref_axis',(1.,0.,0.));
#8912=DIRECTION('center_axis',(0.,1.,0.));
#8913=DIRECTION('ref_axis',(1.,0.,0.));
#8914=DIRECTION('',(0.,1.,0.));
#8915=DIRECTION('center_axis',(0.,-1.,0.));
#8916=DIRECTION('ref_axis',(1.,0.,0.));
#8917=DIRECTION('center_axis',(0.,1.,0.));
#8918=DIRECTION('ref_axis',(1.,0.,0.));
#8919=DIRECTION('center_axis',(0.,1.,0.));
#8920=DIRECTION('ref_axis',(1.,0.,0.));
#8921=DIRECTION('',(0.,1.,0.));
#8922=DIRECTION('center_axis',(0.,-1.,0.));
#8923=DIRECTION('ref_axis',(1.,0.,0.));
#8924=DIRECTION('center_axis',(-1.,0.,0.));
#8925=DIRECTION('ref_axis',(0.,0.,1.));
#8926=DIRECTION('',(0.,0.,-1.));
#8927=DIRECTION('',(0.,1.,0.));
#8928=DIRECTION('',(0.,0.,1.));
#8929=DIRECTION('',(0.,1.,0.));
#8930=DIRECTION('center_axis',(0.233372952475324,0.,-0.972387301980517));
#8931=DIRECTION('ref_axis',(-0.972387301980517,0.,-0.233372952475324));
#8932=DIRECTION('',(0.972387301980517,0.,0.233372952475324));
#8933=DIRECTION('',(-0.972387301980517,0.,-0.233372952475324));
#8934=DIRECTION('',(0.,1.,0.));
#8935=DIRECTION('center_axis',(1.,0.,0.));
#8936=DIRECTION('ref_axis',(0.,0.,-1.));
#8937=DIRECTION('',(0.,0.,1.));
#8938=DIRECTION('',(0.,0.,-1.));
#8939=DIRECTION('',(0.,1.,0.));
#8940=DIRECTION('center_axis',(-0.07974522228289,0.,0.996815278536125));
#8941=DIRECTION('ref_axis',(0.996815278536125,0.,0.07974522228289));
#8942=DIRECTION('',(-0.996815278536125,0.,-0.07974522228289));
#8943=DIRECTION('',(0.996815278536125,0.,0.07974522228289));
#8944=DIRECTION('center_axis',(0.,1.,0.));
#8945=DIRECTION('ref_axis',(0.,0.,1.));
#8946=DIRECTION('center_axis',(0.,1.,0.));
#8947=DIRECTION('ref_axis',(1.,0.,0.));
#8948=DIRECTION('axis',(0.,0.,1.));
#8949=DIRECTION('refdir',(1.,0.,0.));
#8950=DIRECTION('center_axis',(0.,1.,0.));
#8951=DIRECTION('ref_axis',(1.,0.,0.));
#8952=DIRECTION('center_axis',(0.,1.,0.));
#8953=DIRECTION('ref_axis',(1.,0.,0.));
#8954=DIRECTION('',(0.,1.,0.));
#8955=DIRECTION('center_axis',(0.,-1.,0.));
#8956=DIRECTION('ref_axis',(1.,0.,0.));
#8957=DIRECTION('center_axis',(0.,1.,0.));
#8958=DIRECTION('ref_axis',(1.,0.,0.));
#8959=DIRECTION('center_axis',(0.,1.,0.));
#8960=DIRECTION('ref_axis',(1.,0.,0.));
#8961=DIRECTION('',(0.,1.,0.));
#8962=DIRECTION('center_axis',(0.,-1.,0.));
#8963=DIRECTION('ref_axis',(1.,0.,0.));
#8964=DIRECTION('center_axis',(-1.,0.,0.));
#8965=DIRECTION('ref_axis',(0.,0.,1.));
#8966=DIRECTION('',(0.,0.,-1.));
#8967=DIRECTION('',(0.,1.,0.));
#8968=DIRECTION('',(0.,0.,1.));
#8969=DIRECTION('',(0.,1.,0.));
#8970=DIRECTION('center_axis',(0.233372952475324,0.,-0.972387301980517));
#8971=DIRECTION('ref_axis',(-0.972387301980517,0.,-0.233372952475324));
#8972=DIRECTION('',(0.972387301980517,0.,0.233372952475324));
#8973=DIRECTION('',(-0.972387301980517,0.,-0.233372952475324));
#8974=DIRECTION('',(0.,1.,0.));
#8975=DIRECTION('center_axis',(1.,0.,0.));
#8976=DIRECTION('ref_axis',(0.,0.,-1.));
#8977=DIRECTION('',(0.,0.,1.));
#8978=DIRECTION('',(0.,0.,-1.));
#8979=DIRECTION('',(0.,1.,0.));
#8980=DIRECTION('center_axis',(-0.07974522228289,0.,0.996815278536125));
#8981=DIRECTION('ref_axis',(0.996815278536125,0.,0.07974522228289));
#8982=DIRECTION('',(-0.996815278536125,0.,-0.07974522228289));
#8983=DIRECTION('',(0.996815278536125,0.,0.07974522228289));
#8984=DIRECTION('center_axis',(0.,1.,0.));
#8985=DIRECTION('ref_axis',(0.,0.,1.));
#8986=DIRECTION('center_axis',(0.,1.,0.));
#8987=DIRECTION('ref_axis',(1.,0.,0.));
#8988=DIRECTION('axis',(0.,0.,1.));
#8989=DIRECTION('refdir',(1.,0.,0.));
#8990=DIRECTION('center_axis',(0.,1.,0.));
#8991=DIRECTION('ref_axis',(1.,0.,0.));
#8992=DIRECTION('center_axis',(0.,1.,0.));
#8993=DIRECTION('ref_axis',(1.,0.,0.));
#8994=DIRECTION('',(0.,1.,0.));
#8995=DIRECTION('center_axis',(0.,-1.,0.));
#8996=DIRECTION('ref_axis',(1.,0.,0.));
#8997=DIRECTION('center_axis',(0.,1.,0.));
#8998=DIRECTION('ref_axis',(1.,0.,0.));
#8999=DIRECTION('center_axis',(0.,1.,0.));
#9000=DIRECTION('ref_axis',(1.,0.,0.));
#9001=DIRECTION('center_axis',(0.,1.,0.));
#9002=DIRECTION('ref_axis',(1.,0.,0.));
#9003=DIRECTION('',(0.,1.,0.));
#9004=DIRECTION('center_axis',(0.,-1.,0.));
#9005=DIRECTION('ref_axis',(1.,0.,0.));
#9006=DIRECTION('center_axis',(0.,1.,0.));
#9007=DIRECTION('ref_axis',(1.,0.,0.));
#9008=DIRECTION('center_axis',(0.,1.,0.));
#9009=DIRECTION('ref_axis',(1.,0.,0.));
#9010=DIRECTION('center_axis',(0.,1.,0.));
#9011=DIRECTION('ref_axis',(1.,0.,0.));
#9012=DIRECTION('center_axis',(0.,1.,0.));
#9013=DIRECTION('ref_axis',(1.,0.,0.));
#9014=DIRECTION('',(0.,1.,0.));
#9015=DIRECTION('center_axis',(0.,1.,0.));
#9016=DIRECTION('ref_axis',(-1.,0.,0.));
#9017=DIRECTION('',(-1.,0.,0.));
#9018=DIRECTION('',(0.,0.,1.));
#9019=DIRECTION('',(-1.,0.,0.));
#9020=DIRECTION('',(0.,0.,1.));
#9021=DIRECTION('center_axis',(1.,0.,0.));
#9022=DIRECTION('ref_axis',(0.,1.,0.));
#9023=DIRECTION('',(0.,1.,0.));
#9024=DIRECTION('',(0.,1.,0.));
#9025=DIRECTION('',(0.,0.,1.));
#9026=DIRECTION('center_axis',(0.,-1.,0.));
#9027=DIRECTION('ref_axis',(1.,0.,0.));
#9028=DIRECTION('',(1.,0.,0.));
#9029=DIRECTION('',(1.,0.,0.));
#9030=DIRECTION('',(0.,0.,1.));
#9031=DIRECTION('center_axis',(-1.,0.,0.));
#9032=DIRECTION('ref_axis',(0.,-1.,0.));
#9033=DIRECTION('',(0.,-1.,0.));
#9034=DIRECTION('',(0.,-1.,0.));
#9035=DIRECTION('center_axis',(0.,0.,1.));
#9036=DIRECTION('ref_axis',(1.,0.,0.));
#9037=DIRECTION('center_axis',(0.,0.,1.));
#9038=DIRECTION('ref_axis',(1.,0.,0.));
#9039=DIRECTION('axis',(0.,0.,1.));
#9040=DIRECTION('refdir',(1.,0.,0.));
#9041=DIRECTION('center_axis',(0.,1.,0.));
#9042=DIRECTION('ref_axis',(1.,0.,0.));
#9043=DIRECTION('center_axis',(0.,1.,0.));
#9044=DIRECTION('ref_axis',(1.,0.,0.));
#9045=DIRECTION('',(0.,1.,0.));
#9046=DIRECTION('center_axis',(0.,1.,0.));
#9047=DIRECTION('ref_axis',(1.,0.,0.));
#9048=DIRECTION('center_axis',(0.,1.,0.));
#9049=DIRECTION('ref_axis',(1.,0.,0.));
#9050=DIRECTION('center_axis',(0.,1.,0.));
#9051=DIRECTION('ref_axis',(1.,0.,0.));
#9052=DIRECTION('center_axis',(0.,1.,0.));
#9053=DIRECTION('ref_axis',(1.,0.,0.));
#9054=DIRECTION('',(0.,1.,0.));
#9055=DIRECTION('center_axis',(0.,1.,0.));
#9056=DIRECTION('ref_axis',(1.,0.,0.));
#9057=DIRECTION('center_axis',(0.,1.,0.));
#9058=DIRECTION('ref_axis',(1.,0.,0.));
#9059=DIRECTION('center_axis',(0.,-1.,0.));
#9060=DIRECTION('ref_axis',(1.,0.,0.));
#9061=DIRECTION('center_axis',(0.,1.,0.));
#9062=DIRECTION('ref_axis',(1.,0.,0.));
#9063=DIRECTION('',(0.,1.,0.));
#9064=DIRECTION('center_axis',(0.,-1.,0.));
#9065=DIRECTION('ref_axis',(1.,0.,0.));
#9066=DIRECTION('center_axis',(0.,1.,0.));
#9067=DIRECTION('ref_axis',(-1.,0.,0.));
#9068=DIRECTION('',(-1.,0.,0.));
#9069=DIRECTION('',(0.,0.,1.));
#9070=DIRECTION('',(-1.,0.,0.));
#9071=DIRECTION('',(0.,0.,1.));
#9072=DIRECTION('center_axis',(1.,0.,0.));
#9073=DIRECTION('ref_axis',(0.,1.,0.));
#9074=DIRECTION('',(0.,1.,0.));
#9075=DIRECTION('',(0.,1.,0.));
#9076=DIRECTION('',(0.,0.,1.));
#9077=DIRECTION('center_axis',(0.,-1.,0.));
#9078=DIRECTION('ref_axis',(1.,0.,0.));
#9079=DIRECTION('',(1.,0.,0.));
#9080=DIRECTION('',(1.,0.,0.));
#9081=DIRECTION('',(0.,0.,1.));
#9082=DIRECTION('center_axis',(-1.,0.,0.));
#9083=DIRECTION('ref_axis',(0.,-1.,0.));
#9084=DIRECTION('',(0.,-1.,0.));
#9085=DIRECTION('',(0.,-1.,0.));
#9086=DIRECTION('center_axis',(0.,0.,1.));
#9087=DIRECTION('ref_axis',(1.,0.,0.));
#9088=DIRECTION('center_axis',(0.,0.,1.));
#9089=DIRECTION('ref_axis',(1.,0.,0.));
#9090=DIRECTION('axis',(0.,0.,1.));
#9091=DIRECTION('refdir',(1.,0.,0.));
#9092=DIRECTION('center_axis',(0.,1.,0.));
#9093=DIRECTION('ref_axis',(1.,0.,0.));
#9094=DIRECTION('center_axis',(0.,1.,0.));
#9095=DIRECTION('ref_axis',(1.,0.,0.));
#9096=DIRECTION('',(0.,1.,0.));
#9097=DIRECTION('center_axis',(0.,-1.,0.));
#9098=DIRECTION('ref_axis',(1.,0.,0.));
#9099=DIRECTION('center_axis',(0.,1.,0.));
#9100=DIRECTION('ref_axis',(1.,0.,0.));
#9101=DIRECTION('center_axis',(0.,1.,0.));
#9102=DIRECTION('ref_axis',(1.,0.,0.));
#9103=DIRECTION('center_axis',(0.,1.,0.));
#9104=DIRECTION('ref_axis',(1.,0.,0.));
#9105=DIRECTION('',(0.,1.,0.));
#9106=DIRECTION('center_axis',(0.,-1.,0.));
#9107=DIRECTION('ref_axis',(1.,0.,0.));
#9108=DIRECTION('center_axis',(0.,1.,0.));
#9109=DIRECTION('ref_axis',(1.,0.,0.));
#9110=DIRECTION('center_axis',(0.,1.,0.));
#9111=DIRECTION('ref_axis',(1.,0.,0.));
#9112=DIRECTION('center_axis',(0.,1.,0.));
#9113=DIRECTION('ref_axis',(1.,0.,0.));
#9114=DIRECTION('center_axis',(0.,1.,0.));
#9115=DIRECTION('ref_axis',(1.,0.,0.));
#9116=DIRECTION('',(0.,1.,0.));
#9117=DIRECTION('center_axis',(0.,1.,0.));
#9118=DIRECTION('ref_axis',(-1.,0.,0.));
#9119=DIRECTION('',(-1.,0.,0.));
#9120=DIRECTION('',(0.,0.,1.));
#9121=DIRECTION('',(-1.,0.,0.));
#9122=DIRECTION('',(0.,0.,1.));
#9123=DIRECTION('center_axis',(1.,0.,0.));
#9124=DIRECTION('ref_axis',(0.,1.,0.));
#9125=DIRECTION('',(0.,1.,0.));
#9126=DIRECTION('',(0.,1.,0.));
#9127=DIRECTION('',(0.,0.,1.));
#9128=DIRECTION('center_axis',(0.,-1.,0.));
#9129=DIRECTION('ref_axis',(1.,0.,0.));
#9130=DIRECTION('',(1.,0.,0.));
#9131=DIRECTION('',(1.,0.,0.));
#9132=DIRECTION('',(0.,0.,1.));
#9133=DIRECTION('center_axis',(-1.,0.,0.));
#9134=DIRECTION('ref_axis',(0.,-1.,0.));
#9135=DIRECTION('',(0.,-1.,0.));
#9136=DIRECTION('',(0.,-1.,0.));
#9137=DIRECTION('center_axis',(0.,0.,1.));
#9138=DIRECTION('ref_axis',(1.,0.,0.));
#9139=DIRECTION('center_axis',(0.,0.,1.));
#9140=DIRECTION('ref_axis',(1.,0.,0.));
#9141=DIRECTION('axis',(0.,0.,1.));
#9142=DIRECTION('refdir',(1.,0.,0.));
#9143=DIRECTION('center_axis',(0.,1.,0.));
#9144=DIRECTION('ref_axis',(1.,0.,0.));
#9145=DIRECTION('center_axis',(0.,1.,0.));
#9146=DIRECTION('ref_axis',(1.,0.,0.));
#9147=DIRECTION('',(0.,1.,0.));
#9148=DIRECTION('center_axis',(0.,1.,0.));
#9149=DIRECTION('ref_axis',(1.,0.,0.));
#9150=DIRECTION('center_axis',(0.,1.,0.));
#9151=DIRECTION('ref_axis',(1.,0.,0.));
#9152=DIRECTION('center_axis',(0.,1.,0.));
#9153=DIRECTION('ref_axis',(1.,0.,0.));
#9154=DIRECTION('center_axis',(0.,1.,0.));
#9155=DIRECTION('ref_axis',(1.,0.,0.));
#9156=DIRECTION('',(0.,1.,0.));
#9157=DIRECTION('center_axis',(0.,1.,0.));
#9158=DIRECTION('ref_axis',(1.,0.,0.));
#9159=DIRECTION('center_axis',(0.,1.,0.));
#9160=DIRECTION('ref_axis',(1.,0.,0.));
#9161=DIRECTION('center_axis',(0.,-1.,0.));
#9162=DIRECTION('ref_axis',(1.,0.,0.));
#9163=DIRECTION('center_axis',(0.,1.,0.));
#9164=DIRECTION('ref_axis',(1.,0.,0.));
#9165=DIRECTION('',(0.,1.,0.));
#9166=DIRECTION('center_axis',(0.,-1.,0.));
#9167=DIRECTION('ref_axis',(1.,0.,0.));
#9168=DIRECTION('center_axis',(0.,1.,0.));
#9169=DIRECTION('ref_axis',(-1.,0.,0.));
#9170=DIRECTION('',(-1.,0.,0.));
#9171=DIRECTION('',(0.,0.,1.));
#9172=DIRECTION('',(-1.,0.,0.));
#9173=DIRECTION('',(0.,0.,1.));
#9174=DIRECTION('center_axis',(1.,0.,0.));
#9175=DIRECTION('ref_axis',(0.,1.,0.));
#9176=DIRECTION('',(0.,1.,0.));
#9177=DIRECTION('',(0.,1.,0.));
#9178=DIRECTION('',(0.,0.,1.));
#9179=DIRECTION('center_axis',(0.,-1.,0.));
#9180=DIRECTION('ref_axis',(1.,0.,0.));
#9181=DIRECTION('',(1.,0.,0.));
#9182=DIRECTION('',(1.,0.,0.));
#9183=DIRECTION('',(0.,0.,1.));
#9184=DIRECTION('center_axis',(-1.,0.,0.));
#9185=DIRECTION('ref_axis',(0.,-1.,0.));
#9186=DIRECTION('',(0.,-1.,0.));
#9187=DIRECTION('',(0.,-1.,0.));
#9188=DIRECTION('center_axis',(0.,0.,1.));
#9189=DIRECTION('ref_axis',(1.,0.,0.));
#9190=DIRECTION('center_axis',(0.,0.,1.));
#9191=DIRECTION('ref_axis',(1.,0.,0.));
#9192=DIRECTION('axis',(0.,0.,1.));
#9193=DIRECTION('refdir',(1.,0.,0.));
#9194=DIRECTION('center_axis',(0.,0.,-1.));
#9195=DIRECTION('ref_axis',(0.,1.,0.));
#9196=DIRECTION('',(0.,-1.,0.));
#9197=DIRECTION('',(1.,0.,0.));
#9198=DIRECTION('',(0.,1.,0.));
#9199=DIRECTION('',(1.,0.,0.));
#9200=DIRECTION('center_axis',(0.,-1.,0.));
#9201=DIRECTION('ref_axis',(0.,0.,-1.));
#9202=DIRECTION('',(0.,0.,1.));
#9203=DIRECTION('',(0.,0.,-1.));
#9204=DIRECTION('',(1.,0.,0.));
#9205=DIRECTION('center_axis',(0.,0.,1.));
#9206=DIRECTION('ref_axis',(0.,-1.,0.));
#9207=DIRECTION('',(0.,1.,0.));
#9208=DIRECTION('',(0.,-1.,0.));
#9209=DIRECTION('',(1.,0.,0.));
#9210=DIRECTION('center_axis',(0.,1.,0.));
#9211=DIRECTION('ref_axis',(0.,0.,1.));
#9212=DIRECTION('',(0.,0.,-1.));
#9213=DIRECTION('',(0.,0.,1.));
#9214=DIRECTION('center_axis',(0.,0.,1.));
#9215=DIRECTION('ref_axis',(0.,-1.,0.));
#9216=DIRECTION('',(0.,-1.,0.));
#9217=DIRECTION('',(1.,0.,0.));
#9218=DIRECTION('',(0.,-1.,0.));
#9219=DIRECTION('',(1.,0.,0.));
#9220=DIRECTION('center_axis',(0.,1.,0.));
#9221=DIRECTION('ref_axis',(0.,0.,1.));
#9222=DIRECTION('',(0.,0.,1.));
#9223=DIRECTION('',(0.,0.,1.));
#9224=DIRECTION('',(1.,0.,0.));
#9225=DIRECTION('center_axis',(0.,0.,-1.));
#9226=DIRECTION('ref_axis',(0.,1.,0.));
#9227=DIRECTION('',(0.,1.,0.));
#9228=DIRECTION('',(0.,1.,0.));
#9229=DIRECTION('',(1.,0.,0.));
#9230=DIRECTION('center_axis',(0.,-1.,0.));
#9231=DIRECTION('ref_axis',(0.,0.,-1.));
#9232=DIRECTION('',(0.,0.,-1.));
#9233=DIRECTION('',(0.,0.,-1.));
#9234=DIRECTION('center_axis',(1.,0.,0.));
#9235=DIRECTION('ref_axis',(0.,0.,-1.));
#9236=DIRECTION('center_axis',(1.,0.,0.));
#9237=DIRECTION('ref_axis',(0.,0.,-1.));
#9238=DIRECTION('axis',(0.,0.,1.));
#9239=DIRECTION('refdir',(1.,0.,0.));
#9240=DIRECTION('center_axis',(0.,0.,-1.));
#9241=DIRECTION('ref_axis',(0.,1.,0.));
#9242=DIRECTION('',(0.,-1.,0.));
#9243=DIRECTION('',(1.,0.,0.));
#9244=DIRECTION('',(0.,1.,0.));
#9245=DIRECTION('',(1.,0.,0.));
#9246=DIRECTION('center_axis',(0.,-1.,0.));
#9247=DIRECTION('ref_axis',(0.,0.,-1.));
#9248=DIRECTION('',(0.,0.,1.));
#9249=DIRECTION('',(0.,0.,-1.));
#9250=DIRECTION('',(1.,0.,0.));
#9251=DIRECTION('center_axis',(0.,0.,1.));
#9252=DIRECTION('ref_axis',(0.,-1.,0.));
#9253=DIRECTION('',(0.,1.,0.));
#9254=DIRECTION('',(0.,-1.,0.));
#9255=DIRECTION('',(1.,0.,0.));
#9256=DIRECTION('center_axis',(0.,1.,0.));
#9257=DIRECTION('ref_axis',(0.,0.,1.));
#9258=DIRECTION('',(0.,0.,-1.));
#9259=DIRECTION('',(0.,0.,1.));
#9260=DIRECTION('center_axis',(0.,0.,1.));
#9261=DIRECTION('ref_axis',(0.,-1.,0.));
#9262=DIRECTION('',(0.,-1.,0.));
#9263=DIRECTION('',(1.,0.,0.));
#9264=DIRECTION('',(0.,-1.,0.));
#9265=DIRECTION('',(1.,0.,0.));
#9266=DIRECTION('center_axis',(0.,1.,0.));
#9267=DIRECTION('ref_axis',(0.,0.,1.));
#9268=DIRECTION('',(0.,0.,1.));
#9269=DIRECTION('',(0.,0.,1.));
#9270=DIRECTION('',(1.,0.,0.));
#9271=DIRECTION('center_axis',(0.,0.,-1.));
#9272=DIRECTION('ref_axis',(0.,1.,0.));
#9273=DIRECTION('',(0.,1.,0.));
#9274=DIRECTION('',(0.,1.,0.));
#9275=DIRECTION('',(1.,0.,0.));
#9276=DIRECTION('center_axis',(0.,-1.,0.));
#9277=DIRECTION('ref_axis',(0.,0.,-1.));
#9278=DIRECTION('',(0.,0.,-1.));
#9279=DIRECTION('',(0.,0.,-1.));
#9280=DIRECTION('center_axis',(1.,0.,0.));
#9281=DIRECTION('ref_axis',(0.,0.,-1.));
#9282=DIRECTION('center_axis',(1.,0.,0.));
#9283=DIRECTION('ref_axis',(0.,0.,-1.));
#9284=DIRECTION('axis',(0.,0.,1.));
#9285=DIRECTION('refdir',(1.,0.,0.));
#9286=DIRECTION('center_axis',(1.,0.,0.));
#9287=DIRECTION('ref_axis',(0.,0.,-1.));
#9288=DIRECTION('center_axis',(1.,0.,0.));
#9289=DIRECTION('ref_axis',(0.,0.,-1.));
#9290=DIRECTION('',(1.,0.,0.));
#9291=DIRECTION('center_axis',(-1.,0.,0.));
#9292=DIRECTION('ref_axis',(0.,0.,-1.));
#9293=DIRECTION('center_axis',(1.,0.,0.));
#9294=DIRECTION('ref_axis',(0.,0.,-1.));
#9295=DIRECTION('center_axis',(1.,0.,0.));
#9296=DIRECTION('ref_axis',(0.,0.,-1.));
#9297=DIRECTION('',(1.,0.,0.));
#9298=DIRECTION('center_axis',(-1.,0.,0.));
#9299=DIRECTION('ref_axis',(0.,0.,-1.));
#9300=DIRECTION('center_axis',(1.,0.,0.));
#9301=DIRECTION('ref_axis',(0.,0.,-1.));
#9302=DIRECTION('center_axis',(1.,0.,0.));
#9303=DIRECTION('ref_axis',(0.,0.,-1.));
#9304=DIRECTION('',(1.,0.,0.));
#9305=DIRECTION('center_axis',(-1.,0.,0.));
#9306=DIRECTION('ref_axis',(0.,0.,-1.));
#9307=DIRECTION('center_axis',(1.,0.,0.));
#9308=DIRECTION('ref_axis',(0.,0.,-1.));
#9309=DIRECTION('center_axis',(1.,0.,0.));
#9310=DIRECTION('ref_axis',(0.,0.,-1.));
#9311=DIRECTION('',(1.,0.,0.));
#9312=DIRECTION('center_axis',(-1.,0.,0.));
#9313=DIRECTION('ref_axis',(0.,0.,-1.));
#9314=DIRECTION('center_axis',(1.,0.,0.));
#9315=DIRECTION('ref_axis',(0.,0.,-1.));
#9316=DIRECTION('center_axis',(1.,0.,0.));
#9317=DIRECTION('ref_axis',(0.,0.,-1.));
#9318=DIRECTION('',(1.,0.,0.));
#9319=DIRECTION('center_axis',(-1.,0.,0.));
#9320=DIRECTION('ref_axis',(0.,0.,-1.));
#9321=DIRECTION('center_axis',(1.,0.,0.));
#9322=DIRECTION('ref_axis',(0.,0.,-1.));
#9323=DIRECTION('center_axis',(1.,0.,0.));
#9324=DIRECTION('ref_axis',(0.,0.,-1.));
#9325=DIRECTION('',(1.,0.,0.));
#9326=DIRECTION('center_axis',(-1.,0.,0.));
#9327=DIRECTION('ref_axis',(0.,0.,-1.));
#9328=DIRECTION('center_axis',(1.,0.,0.));
#9329=DIRECTION('ref_axis',(0.,0.,-1.));
#9330=DIRECTION('center_axis',(1.,0.,0.));
#9331=DIRECTION('ref_axis',(0.,0.,-1.));
#9332=DIRECTION('',(1.,0.,0.));
#9333=DIRECTION('center_axis',(-1.,0.,0.));
#9334=DIRECTION('ref_axis',(0.,0.,-1.));
#9335=DIRECTION('center_axis',(1.,0.,0.));
#9336=DIRECTION('ref_axis',(0.,0.,-1.));
#9337=DIRECTION('center_axis',(1.,0.,0.));
#9338=DIRECTION('ref_axis',(0.,0.,-1.));
#9339=DIRECTION('',(1.,0.,0.));
#9340=DIRECTION('center_axis',(-1.,0.,0.));
#9341=DIRECTION('ref_axis',(0.,0.,-1.));
#9342=DIRECTION('center_axis',(0.,1.,0.));
#9343=DIRECTION('ref_axis',(-1.,0.,0.));
#9344=DIRECTION('',(-1.,0.,0.));
#9345=DIRECTION('',(0.,0.,1.));
#9346=DIRECTION('',(-1.,0.,0.));
#9347=DIRECTION('',(0.,0.,1.));
#9348=DIRECTION('center_axis',(1.,0.,0.));
#9349=DIRECTION('ref_axis',(0.,1.,0.));
#9350=DIRECTION('',(0.,1.,0.));
#9351=DIRECTION('',(0.,1.,0.));
#9352=DIRECTION('',(0.,0.,1.));
#9353=DIRECTION('center_axis',(0.,-1.,0.));
#9354=DIRECTION('ref_axis',(1.,0.,0.));
#9355=DIRECTION('',(1.,0.,0.));
#9356=DIRECTION('',(1.,0.,0.));
#9357=DIRECTION('',(0.,0.,1.));
#9358=DIRECTION('center_axis',(-1.,0.,0.));
#9359=DIRECTION('ref_axis',(0.,-1.,0.));
#9360=DIRECTION('',(0.,-1.,0.));
#9361=DIRECTION('',(0.,-1.,0.));
#9362=DIRECTION('center_axis',(0.,0.,1.));
#9363=DIRECTION('ref_axis',(1.,0.,0.));
#9364=DIRECTION('center_axis',(0.,0.,1.));
#9365=DIRECTION('ref_axis',(1.,0.,0.));
#9366=DIRECTION('axis',(0.,0.,1.));
#9367=DIRECTION('refdir',(1.,0.,0.));
#9368=DIRECTION('center_axis',(1.,0.,0.));
#9369=DIRECTION('ref_axis',(0.,0.,-1.));
#9370=DIRECTION('center_axis',(1.,0.,0.));
#9371=DIRECTION('ref_axis',(0.,0.,-1.));
#9372=DIRECTION('',(1.,0.,0.));
#9373=DIRECTION('center_axis',(-1.,0.,0.));
#9374=DIRECTION('ref_axis',(0.,0.,-1.));
#9375=DIRECTION('center_axis',(1.,0.,0.));
#9376=DIRECTION('ref_axis',(0.,0.,-1.));
#9377=DIRECTION('center_axis',(1.,0.,0.));
#9378=DIRECTION('ref_axis',(0.,0.,-1.));
#9379=DIRECTION('',(1.,0.,0.));
#9380=DIRECTION('center_axis',(-1.,0.,0.));
#9381=DIRECTION('ref_axis',(0.,0.,-1.));
#9382=DIRECTION('center_axis',(0.,1.,0.));
#9383=DIRECTION('ref_axis',(-1.,0.,0.));
#9384=DIRECTION('',(-1.,0.,0.));
#9385=DIRECTION('',(0.,0.,1.));
#9386=DIRECTION('',(-1.,0.,0.));
#9387=DIRECTION('',(0.,0.,1.));
#9388=DIRECTION('center_axis',(1.,0.,0.));
#9389=DIRECTION('ref_axis',(0.,1.,0.));
#9390=DIRECTION('',(0.,1.,0.));
#9391=DIRECTION('',(0.,1.,0.));
#9392=DIRECTION('',(0.,0.,1.));
#9393=DIRECTION('center_axis',(0.,1.,0.));
#9394=DIRECTION('ref_axis',(-1.,0.,0.));
#9395=DIRECTION('',(-1.,0.,0.));
#9396=DIRECTION('',(-1.,0.,0.));
#9397=DIRECTION('',(0.,0.,1.));
#9398=DIRECTION('center_axis',(1.,0.,0.));
#9399=DIRECTION('ref_axis',(0.,1.,0.));
#9400=DIRECTION('',(0.,1.,0.));
#9401=DIRECTION('',(0.,1.,0.));
#9402=DIRECTION('',(0.,0.,1.));
#9403=DIRECTION('center_axis',(0.,-1.,0.));
#9404=DIRECTION('ref_axis',(1.,0.,0.));
#9405=DIRECTION('',(1.,0.,0.));
#9406=DIRECTION('',(1.,0.,0.));
#9407=DIRECTION('',(0.,0.,1.));
#9408=DIRECTION('center_axis',(-1.,0.,0.));
#9409=DIRECTION('ref_axis',(0.,-1.,0.));
#9410=DIRECTION('',(0.,-1.,0.));
#9411=DIRECTION('',(0.,-1.,0.));
#9412=DIRECTION('center_axis',(0.,0.,1.));
#9413=DIRECTION('ref_axis',(1.,0.,0.));
#9414=DIRECTION('center_axis',(0.,0.,1.));
#9415=DIRECTION('ref_axis',(1.,0.,0.));
#9416=DIRECTION('axis',(0.,0.,1.));
#9417=DIRECTION('refdir',(1.,0.,0.));
#9418=DIRECTION('center_axis',(1.,0.,0.));
#9419=DIRECTION('ref_axis',(0.,0.,-1.));
#9420=DIRECTION('center_axis',(1.,0.,0.));
#9421=DIRECTION('ref_axis',(0.,0.,-1.));
#9422=DIRECTION('',(1.,0.,0.));
#9423=DIRECTION('center_axis',(1.,0.,0.));
#9424=DIRECTION('ref_axis',(0.,0.,-1.));
#9425=DIRECTION('center_axis',(1.,0.,0.));
#9426=DIRECTION('ref_axis',(0.,0.,-1.));
#9427=DIRECTION('center_axis',(1.,0.,0.));
#9428=DIRECTION('ref_axis',(0.,0.,-1.));
#9429=DIRECTION('center_axis',(1.,0.,0.));
#9430=DIRECTION('ref_axis',(0.,0.,-1.));
#9431=DIRECTION('',(1.,0.,0.));
#9432=DIRECTION('center_axis',(-1.,0.,0.));
#9433=DIRECTION('ref_axis',(0.,0.,-1.));
#9434=DIRECTION('center_axis',(0.,0.,1.));
#9435=DIRECTION('ref_axis',(1.,0.,0.));
#9436=DIRECTION('',(0.,-1.,0.));
#9437=DIRECTION('',(1.,0.,0.));
#9438=DIRECTION('',(0.,1.,0.));
#9439=DIRECTION('',(-1.,0.,0.));
#9440=DIRECTION('center_axis',(-1.,0.,0.));
#9441=DIRECTION('ref_axis',(0.,0.,1.));
#9442=DIRECTION('',(0.,0.,-1.));
#9443=DIRECTION('',(0.,0.,1.));
#9444=DIRECTION('',(0.,1.,0.));
#9445=DIRECTION('center_axis',(0.,1.,0.));
#9446=DIRECTION('ref_axis',(1.,0.,0.));
#9447=DIRECTION('',(0.,0.,-1.));
#9448=DIRECTION('',(1.,0.,0.));
#9449=DIRECTION('center_axis',(0.,1.,0.));
#9450=DIRECTION('ref_axis',(-1.,0.,0.));
#9451=DIRECTION('',(0.,0.,1.));
#9452=DIRECTION('',(-1.,0.,0.));
#9453=DIRECTION('',(0.,0.,1.));
#9454=DIRECTION('',(-1.,0.,0.));
#9455=DIRECTION('center_axis',(0.,0.,1.));
#9456=DIRECTION('ref_axis',(1.,0.,0.));
#9457=DIRECTION('',(0.,1.,0.));
#9458=DIRECTION('',(1.,0.,0.));
#9459=DIRECTION('',(0.,-1.,0.));
#9460=DIRECTION('center_axis',(1.,0.,0.));
#9461=DIRECTION('ref_axis',(0.,1.,0.));
#9462=DIRECTION('',(0.,1.,0.));
#9463=DIRECTION('',(0.,0.,1.));
#9464=DIRECTION('center_axis',(0.,-1.,0.));
#9465=DIRECTION('ref_axis',(1.,0.,0.));
#9466=DIRECTION('',(1.,0.,0.));
#9467=DIRECTION('',(0.,0.,1.));
#9468=DIRECTION('center_axis',(-1.,0.,0.));
#9469=DIRECTION('ref_axis',(0.,-1.,0.));
#9470=DIRECTION('',(0.,-1.,0.));
#9471=DIRECTION('center_axis',(0.,0.,1.));
#9472=DIRECTION('ref_axis',(1.,0.,0.));
#9473=DIRECTION('axis',(0.,0.,1.));
#9474=DIRECTION('refdir',(1.,0.,0.));
#9475=DIRECTION('center_axis',(1.,0.,0.));
#9476=DIRECTION('ref_axis',(0.,0.,-1.));
#9477=DIRECTION('center_axis',(1.,0.,0.));
#9478=DIRECTION('ref_axis',(0.,0.,-1.));
#9479=DIRECTION('',(1.,0.,0.));
#9480=DIRECTION('center_axis',(1.,0.,0.));
#9481=DIRECTION('ref_axis',(0.,0.,-1.));
#9482=DIRECTION('center_axis',(1.,0.,0.));
#9483=DIRECTION('ref_axis',(0.,0.,-1.));
#9484=DIRECTION('center_axis',(1.,0.,0.));
#9485=DIRECTION('ref_axis',(0.,0.,-1.));
#9486=DIRECTION('center_axis',(1.,0.,0.));
#9487=DIRECTION('ref_axis',(0.,0.,-1.));
#9488=DIRECTION('',(1.,0.,0.));
#9489=DIRECTION('center_axis',(-1.,0.,0.));
#9490=DIRECTION('ref_axis',(0.,0.,-1.));
#9491=DIRECTION('center_axis',(0.,0.,1.));
#9492=DIRECTION('ref_axis',(1.,0.,0.));
#9493=DIRECTION('',(0.,-1.,0.));
#9494=DIRECTION('',(1.,0.,0.));
#9495=DIRECTION('',(0.,1.,0.));
#9496=DIRECTION('',(-1.,0.,0.));
#9497=DIRECTION('center_axis',(-1.,0.,0.));
#9498=DIRECTION('ref_axis',(0.,0.,1.));
#9499=DIRECTION('',(0.,0.,-1.));
#9500=DIRECTION('',(0.,0.,1.));
#9501=DIRECTION('',(0.,1.,0.));
#9502=DIRECTION('center_axis',(0.,1.,0.));
#9503=DIRECTION('ref_axis',(1.,0.,0.));
#9504=DIRECTION('',(0.,0.,-1.));
#9505=DIRECTION('',(1.,0.,0.));
#9506=DIRECTION('center_axis',(0.,1.,0.));
#9507=DIRECTION('ref_axis',(-1.,0.,0.));
#9508=DIRECTION('',(0.,0.,1.));
#9509=DIRECTION('',(-1.,0.,0.));
#9510=DIRECTION('',(0.,0.,1.));
#9511=DIRECTION('',(-1.,0.,0.));
#9512=DIRECTION('center_axis',(0.,0.,1.));
#9513=DIRECTION('ref_axis',(1.,0.,0.));
#9514=DIRECTION('',(0.,1.,0.));
#9515=DIRECTION('',(1.,0.,0.));
#9516=DIRECTION('',(0.,-1.,0.));
#9517=DIRECTION('center_axis',(1.,0.,0.));
#9518=DIRECTION('ref_axis',(0.,1.,0.));
#9519=DIRECTION('',(0.,1.,0.));
#9520=DIRECTION('',(0.,0.,1.));
#9521=DIRECTION('center_axis',(0.,-1.,0.));
#9522=DIRECTION('ref_axis',(1.,0.,0.));
#9523=DIRECTION('',(1.,0.,0.));
#9524=DIRECTION('',(0.,0.,1.));
#9525=DIRECTION('center_axis',(-1.,0.,0.));
#9526=DIRECTION('ref_axis',(0.,-1.,0.));
#9527=DIRECTION('',(0.,-1.,0.));
#9528=DIRECTION('center_axis',(0.,0.,1.));
#9529=DIRECTION('ref_axis',(1.,0.,0.));
#9530=DIRECTION('axis',(0.,0.,1.));
#9531=DIRECTION('refdir',(1.,0.,0.));
#9532=DIRECTION('center_axis',(1.,0.,0.));
#9533=DIRECTION('ref_axis',(0.,0.,-1.));
#9534=DIRECTION('center_axis',(1.,0.,0.));
#9535=DIRECTION('ref_axis',(0.,0.,-1.));
#9536=DIRECTION('',(1.,0.,0.));
#9537=DIRECTION('center_axis',(-1.,0.,0.));
#9538=DIRECTION('ref_axis',(0.,0.,-1.));
#9539=DIRECTION('center_axis',(0.,1.,0.));
#9540=DIRECTION('ref_axis',(-1.,0.,0.));
#9541=DIRECTION('',(-1.,0.,0.));
#9542=DIRECTION('',(0.,0.,1.));
#9543=DIRECTION('',(-1.,0.,0.));
#9544=DIRECTION('',(0.,0.,1.));
#9545=DIRECTION('center_axis',(1.,0.,0.));
#9546=DIRECTION('ref_axis',(0.,1.,0.));
#9547=DIRECTION('',(0.,1.,0.));
#9548=DIRECTION('',(0.,1.,0.));
#9549=DIRECTION('',(0.,0.,1.));
#9550=DIRECTION('center_axis',(0.,-1.,0.));
#9551=DIRECTION('ref_axis',(1.,0.,0.));
#9552=DIRECTION('',(1.,0.,0.));
#9553=DIRECTION('',(1.,0.,0.));
#9554=DIRECTION('',(0.,0.,1.));
#9555=DIRECTION('center_axis',(-1.,0.,0.));
#9556=DIRECTION('ref_axis',(0.,-1.,0.));
#9557=DIRECTION('',(0.,-1.,0.));
#9558=DIRECTION('',(0.,-1.,0.));
#9559=DIRECTION('center_axis',(0.,0.,1.));
#9560=DIRECTION('ref_axis',(1.,0.,0.));
#9561=DIRECTION('center_axis',(0.,0.,1.));
#9562=DIRECTION('ref_axis',(1.,0.,0.));
#9563=DIRECTION('axis',(0.,0.,1.));
#9564=DIRECTION('refdir',(1.,0.,0.));
#9565=DIRECTION('center_axis',(1.,0.,0.));
#9566=DIRECTION('ref_axis',(0.,0.,-1.));
#9567=DIRECTION('center_axis',(1.,0.,0.));
#9568=DIRECTION('ref_axis',(0.,0.,-1.));
#9569=DIRECTION('',(1.,0.,0.));
#9570=DIRECTION('center_axis',(-1.,0.,0.));
#9571=DIRECTION('ref_axis',(0.,0.,-1.));
#9572=DIRECTION('center_axis',(0.,1.,0.));
#9573=DIRECTION('ref_axis',(-1.,0.,0.));
#9574=DIRECTION('',(-1.,0.,0.));
#9575=DIRECTION('',(0.,0.,1.));
#9576=DIRECTION('',(-1.,0.,0.));
#9577=DIRECTION('',(0.,0.,1.));
#9578=DIRECTION('center_axis',(1.,0.,0.));
#9579=DIRECTION('ref_axis',(0.,1.,0.));
#9580=DIRECTION('',(0.,1.,0.));
#9581=DIRECTION('',(0.,1.,0.));
#9582=DIRECTION('',(0.,0.,1.));
#9583=DIRECTION('center_axis',(0.,-1.,0.));
#9584=DIRECTION('ref_axis',(1.,0.,0.));
#9585=DIRECTION('',(1.,0.,0.));
#9586=DIRECTION('',(1.,0.,0.));
#9587=DIRECTION('',(0.,0.,1.));
#9588=DIRECTION('center_axis',(-1.,0.,0.));
#9589=DIRECTION('ref_axis',(0.,-1.,0.));
#9590=DIRECTION('',(0.,-1.,0.));
#9591=DIRECTION('',(0.,-1.,0.));
#9592=DIRECTION('center_axis',(0.,0.,1.));
#9593=DIRECTION('ref_axis',(1.,0.,0.));
#9594=DIRECTION('center_axis',(0.,0.,1.));
#9595=DIRECTION('ref_axis',(1.,0.,0.));
#9596=DIRECTION('axis',(0.,0.,1.));
#9597=DIRECTION('refdir',(1.,0.,0.));
#9598=DIRECTION('center_axis',(0.,0.,-1.));
#9599=DIRECTION('ref_axis',(0.,1.,0.));
#9600=DIRECTION('',(0.,1.,0.));
#9601=DIRECTION('',(1.,0.,0.));
#9602=DIRECTION('',(0.,-1.,0.));
#9603=DIRECTION('',(1.,0.,0.));
#9604=DIRECTION('center_axis',(0.,1.,-8.88178419700125E-16));
#9605=DIRECTION('ref_axis',(0.,8.88178419700125E-16,1.));
#9606=DIRECTION('',(0.,8.88178419700125E-16,1.));
#9607=DIRECTION('',(1.,0.,0.));
#9608=DIRECTION('',(0.,-8.88178419700125E-16,-1.));
#9609=DIRECTION('center_axis',(0.,-7.40148683083439E-16,-1.));
#9610=DIRECTION('ref_axis',(0.,1.,-7.40148683083439E-16));
#9611=DIRECTION('',(0.,1.,-7.40148683083439E-16));
#9612=DIRECTION('',(1.,0.,0.));
#9613=DIRECTION('',(0.,-1.,7.40148683083439E-16));
#9614=DIRECTION('center_axis',(0.,-0.707106781186547,-0.707106781186548));
#9615=DIRECTION('ref_axis',(0.,0.707106781186548,-0.707106781186547));
#9616=DIRECTION('',(0.,0.707106781186548,-0.707106781186547));
#9617=DIRECTION('',(1.,0.,0.));
#9618=DIRECTION('',(0.,-0.707106781186548,0.707106781186547));
#9619=DIRECTION('center_axis',(0.,-1.,2.77555756156289E-16));
#9620=DIRECTION('ref_axis',(0.,-2.77555756156289E-16,-1.));
#9621=DIRECTION('',(0.,-2.77555756156289E-16,-1.));
#9622=DIRECTION('',(1.,0.,0.));
#9623=DIRECTION('',(0.,2.77555756156289E-16,1.));
#9624=DIRECTION('center_axis',(0.,-0.707106781186547,0.707106781186548));
#9625=DIRECTION('ref_axis',(0.,-0.707106781186548,-0.707106781186547));
#9626=DIRECTION('',(0.,-0.707106781186548,-0.707106781186547));
#9627=DIRECTION('',(1.,0.,0.));
#9628=DIRECTION('',(0.,0.707106781186548,0.707106781186547));
#9629=DIRECTION('center_axis',(0.,7.40148683083438E-16,1.));
#9630=DIRECTION('ref_axis',(0.,-1.,7.40148683083438E-16));
#9631=DIRECTION('',(0.,-1.,7.40148683083438E-16));
#9632=DIRECTION('',(1.,0.,0.));
#9633=DIRECTION('',(0.,1.,-7.40148683083438E-16));
#9634=DIRECTION('center_axis',(0.,1.,-4.44089209850063E-16));
#9635=DIRECTION('ref_axis',(0.,4.44089209850063E-16,1.));
#9636=DIRECTION('',(0.,4.44089209850063E-16,1.));
#9637=DIRECTION('',(1.,0.,0.));
#9638=DIRECTION('',(0.,-4.44089209850063E-16,-1.));
#9639=DIRECTION('center_axis',(0.,2.41352831440251E-16,1.));
#9640=DIRECTION('ref_axis',(0.,-1.,2.41352831440251E-16));
#9641=DIRECTION('',(0.,-1.,2.41352831440251E-16));
#9642=DIRECTION('',(-1.,0.,0.));
#9643=DIRECTION('',(0.,1.,-2.41352831440251E-16));
#9644=DIRECTION('center_axis',(0.,-1.,2.41352831440251E-16));
#9645=DIRECTION('ref_axis',(0.,-2.41352831440251E-16,-1.));
#9646=DIRECTION('',(0.,-2.41352831440251E-16,-1.));
#9647=DIRECTION('',(1.,0.,0.));
#9648=DIRECTION('',(0.,2.41352831440251E-16,1.));
#9649=DIRECTION('',(1.,0.,0.));
#9650=DIRECTION('center_axis',(0.,0.,-1.));
#9651=DIRECTION('ref_axis',(0.,1.,0.));
#9652=DIRECTION('',(0.,1.,0.));
#9653=DIRECTION('',(1.,0.,0.));
#9654=DIRECTION('',(0.,-1.,0.));
#9655=DIRECTION('center_axis',(0.,-1.,0.));
#9656=DIRECTION('ref_axis',(0.,0.,-1.));
#9657=DIRECTION('',(0.,0.,-1.));
#9658=DIRECTION('',(1.,0.,0.));
#9659=DIRECTION('',(0.,0.,1.));
#9660=DIRECTION('center_axis',(0.,-0.707106781186547,0.707106781186548));
#9661=DIRECTION('ref_axis',(0.,-0.707106781186548,-0.707106781186547));
#9662=DIRECTION('',(0.,-0.707106781186548,-0.707106781186547));
#9663=DIRECTION('',(1.,0.,0.));
#9664=DIRECTION('',(0.,0.707106781186548,0.707106781186547));
#9665=DIRECTION('center_axis',(0.,0.,1.));
#9666=DIRECTION('ref_axis',(0.,-1.,0.));
#9667=DIRECTION('',(0.,-1.,0.));
#9668=DIRECTION('',(1.,0.,0.));
#9669=DIRECTION('',(0.,1.,0.));
#9670=DIRECTION('center_axis',(0.,0.707106781186548,0.707106781186547));
#9671=DIRECTION('ref_axis',(0.,-0.707106781186547,0.707106781186548));
#9672=DIRECTION('',(0.,-0.707106781186547,0.707106781186548));
#9673=DIRECTION('',(1.,0.,0.));
#9674=DIRECTION('',(0.,0.707106781186547,-0.707106781186548));
#9675=DIRECTION('center_axis',(0.,1.,0.));
#9676=DIRECTION('ref_axis',(0.,0.,1.));
#9677=DIRECTION('',(0.,0.,1.));
#9678=DIRECTION('',(1.,0.,0.));
#9679=DIRECTION('',(0.,0.,-1.));
#9680=DIRECTION('center_axis',(0.,0.,-1.));
#9681=DIRECTION('ref_axis',(0.,1.,0.));
#9682=DIRECTION('',(0.,1.,0.));
#9683=DIRECTION('',(1.,0.,0.));
#9684=DIRECTION('',(0.,-1.,0.));
#9685=DIRECTION('center_axis',(0.,1.,-2.41352831440251E-16));
#9686=DIRECTION('ref_axis',(0.,2.41352831440251E-16,1.));
#9687=DIRECTION('',(0.,2.41352831440251E-16,1.));
#9688=DIRECTION('',(-1.,0.,0.));
#9689=DIRECTION('',(0.,-2.41352831440251E-16,-1.));
#9690=DIRECTION('center_axis',(0.,0.,1.));
#9691=DIRECTION('ref_axis',(0.,-1.,0.));
#9692=DIRECTION('',(0.,-1.,0.));
#9693=DIRECTION('',(1.,0.,0.));
#9694=DIRECTION('',(0.,1.,0.));
#9695=DIRECTION('',(1.,0.,0.));
#9696=DIRECTION('center_axis',(0.,-1.,0.));
#9697=DIRECTION('ref_axis',(0.,0.,-1.));
#9698=DIRECTION('',(0.,0.,-1.));
#9699=DIRECTION('',(1.,0.,0.));
#9700=DIRECTION('',(0.,0.,1.));
#9701=DIRECTION('center_axis',(0.,0.,1.));
#9702=DIRECTION('ref_axis',(0.,-1.,0.));
#9703=DIRECTION('',(0.,-1.,0.));
#9704=DIRECTION('',(1.,0.,0.));
#9705=DIRECTION('',(0.,1.,0.));
#9706=DIRECTION('center_axis',(0.,0.707106781186548,0.707106781186548));
#9707=DIRECTION('ref_axis',(0.,-0.707106781186548,0.707106781186548));
#9708=DIRECTION('',(0.,-0.707106781186548,0.707106781186548));
#9709=DIRECTION('',(1.,0.,0.));
#9710=DIRECTION('',(0.,0.707106781186548,-0.707106781186548));
#9711=DIRECTION('center_axis',(0.,1.,0.));
#9712=DIRECTION('ref_axis',(0.,0.,1.));
#9713=DIRECTION('',(0.,0.,1.));
#9714=DIRECTION('',(1.,0.,0.));
#9715=DIRECTION('',(0.,0.,-1.));
#9716=DIRECTION('center_axis',(0.,0.707106781186548,-0.707106781186547));
#9717=DIRECTION('ref_axis',(0.,0.707106781186547,0.707106781186548));
#9718=DIRECTION('',(0.,0.707106781186547,0.707106781186548));
#9719=DIRECTION('',(1.,0.,0.));
#9720=DIRECTION('',(0.,-0.707106781186547,-0.707106781186548));
#9721=DIRECTION('center_axis',(0.,-7.40148683083438E-16,-1.));
#9722=DIRECTION('ref_axis',(0.,1.,-7.40148683083438E-16));
#9723=DIRECTION('',(0.,1.,-7.40148683083438E-16));
#9724=DIRECTION('',(1.,0.,0.));
#9725=DIRECTION('',(0.,-1.,7.40148683083438E-16));
#9726=DIRECTION('center_axis',(0.,-1.,0.));
#9727=DIRECTION('ref_axis',(0.,0.,-1.));
#9728=DIRECTION('',(0.,0.,-1.));
#9729=DIRECTION('',(1.,0.,0.));
#9730=DIRECTION('',(0.,0.,1.));
#9731=DIRECTION('center_axis',(0.,0.,-1.));
#9732=DIRECTION('ref_axis',(0.,1.,0.));
#9733=DIRECTION('',(0.,1.,0.));
#9734=DIRECTION('',(-1.,0.,0.));
#9735=DIRECTION('',(0.,-1.,0.));
#9736=DIRECTION('center_axis',(0.,1.,0.));
#9737=DIRECTION('ref_axis',(0.,0.,1.));
#9738=DIRECTION('',(0.,0.,1.));
#9739=DIRECTION('',(1.,0.,0.));
#9740=DIRECTION('',(0.,0.,-1.));
#9741=DIRECTION('',(1.,0.,0.));
#9742=DIRECTION('center_axis',(0.,0.,1.));
#9743=DIRECTION('ref_axis',(0.,-1.,0.));
#9744=DIRECTION('',(0.,-1.,0.));
#9745=DIRECTION('',(1.,0.,0.));
#9746=DIRECTION('',(0.,1.,0.));
#9747=DIRECTION('center_axis',(0.,1.,0.));
#9748=DIRECTION('ref_axis',(0.,0.,1.));
#9749=DIRECTION('',(0.,0.,1.));
#9750=DIRECTION('',(1.,0.,0.));
#9751=DIRECTION('',(0.,0.,-1.));
#9752=DIRECTION('center_axis',(0.,0.707106781186547,-0.707106781186548));
#9753=DIRECTION('ref_axis',(0.,0.707106781186548,0.707106781186547));
#9754=DIRECTION('',(0.,0.707106781186548,0.707106781186547));
#9755=DIRECTION('',(1.,0.,0.));
#9756=DIRECTION('',(0.,-0.707106781186548,-0.707106781186547));
#9757=DIRECTION('center_axis',(0.,0.,-1.));
#9758=DIRECTION('ref_axis',(0.,1.,0.));
#9759=DIRECTION('',(0.,1.,0.));
#9760=DIRECTION('',(1.,0.,0.));
#9761=DIRECTION('',(0.,-1.,0.));
#9762=DIRECTION('center_axis',(0.,-0.707106781186547,-0.707106781186548));
#9763=DIRECTION('ref_axis',(0.,0.707106781186548,-0.707106781186547));
#9764=DIRECTION('',(0.,0.707106781186548,-0.707106781186547));
#9765=DIRECTION('',(1.,0.,0.));
#9766=DIRECTION('',(0.,-0.707106781186548,0.707106781186547));
#9767=DIRECTION('center_axis',(0.,-1.,0.));
#9768=DIRECTION('ref_axis',(0.,0.,-1.));
#9769=DIRECTION('',(0.,0.,-1.));
#9770=DIRECTION('',(1.,0.,0.));
#9771=DIRECTION('',(0.,0.,1.));
#9772=DIRECTION('center_axis',(0.,0.,1.));
#9773=DIRECTION('ref_axis',(0.,-1.,0.));
#9774=DIRECTION('',(0.,-1.,0.));
#9775=DIRECTION('',(1.,0.,0.));
#9776=DIRECTION('',(0.,1.,0.));
#9777=DIRECTION('center_axis',(0.,-1.,0.));
#9778=DIRECTION('ref_axis',(0.,0.,-1.));
#9779=DIRECTION('',(0.,0.,-1.));
#9780=DIRECTION('',(-1.,0.,0.));
#9781=DIRECTION('',(0.,0.,1.));
#9782=DIRECTION('center_axis',(1.,0.,0.));
#9783=DIRECTION('ref_axis',(0.,0.,-1.));
#9784=DIRECTION('center_axis',(1.,0.,0.));
#9785=DIRECTION('ref_axis',(0.,0.,-1.));
#9786=DIRECTION('',(1.,0.,0.));
#9787=DIRECTION('center_axis',(-1.,0.,0.));
#9788=DIRECTION('ref_axis',(0.,0.,-1.));
#9789=DIRECTION('center_axis',(0.,1.,0.));
#9790=DIRECTION('ref_axis',(0.,0.,1.));
#9791=DIRECTION('',(0.,0.,1.));
#9792=DIRECTION('',(1.,0.,0.));
#9793=DIRECTION('',(0.,0.,1.));
#9794=DIRECTION('center_axis',(0.,1.,0.));
#9795=DIRECTION('ref_axis',(0.,0.,1.));
#9796=DIRECTION('',(0.,0.,1.));
#9797=DIRECTION('',(1.,0.,0.));
#9798=DIRECTION('',(0.,0.,1.));
#9799=DIRECTION('center_axis',(0.,0.,-1.));
#9800=DIRECTION('ref_axis',(0.,1.,0.));
#9801=DIRECTION('',(0.,1.,0.));
#9802=DIRECTION('',(0.,1.,0.));
#9803=DIRECTION('center_axis',(0.,0.,-1.));
#9804=DIRECTION('ref_axis',(0.,1.,0.));
#9805=DIRECTION('',(0.,1.,0.));
#9806=DIRECTION('',(1.,0.,0.));
#9807=DIRECTION('',(0.,1.,0.));
#9808=DIRECTION('center_axis',(0.,-1.,0.));
#9809=DIRECTION('ref_axis',(0.,0.,-1.));
#9810=DIRECTION('',(0.,0.,-1.));
#9811=DIRECTION('',(0.,0.,-1.));
#9812=DIRECTION('center_axis',(0.,-1.,0.));
#9813=DIRECTION('ref_axis',(0.,0.,-1.));
#9814=DIRECTION('',(0.,0.,-1.));
#9815=DIRECTION('',(1.,0.,0.));
#9816=DIRECTION('',(0.,0.,-1.));
#9817=DIRECTION('center_axis',(0.,0.,1.));
#9818=DIRECTION('ref_axis',(0.,-1.,0.));
#9819=DIRECTION('',(0.,-1.,0.));
#9820=DIRECTION('',(0.,-1.,0.));
#9821=DIRECTION('center_axis',(0.,0.,1.));
#9822=DIRECTION('ref_axis',(0.,-1.,0.));
#9823=DIRECTION('',(0.,-1.,0.));
#9824=DIRECTION('',(0.,-1.,0.));
#9825=DIRECTION('center_axis',(1.,0.,0.));
#9826=DIRECTION('ref_axis',(0.,0.,-1.));
#9827=DIRECTION('center_axis',(1.,0.,0.));
#9828=DIRECTION('ref_axis',(0.,0.,-1.));
#9829=DIRECTION('axis',(0.,0.,1.));
#9830=DIRECTION('refdir',(1.,0.,0.));
#9831=DIRECTION('center_axis',(0.,1.,0.));
#9832=DIRECTION('ref_axis',(0.,0.,1.));
#9833=DIRECTION('center_axis',(0.,-1.,0.));
#9834=DIRECTION('ref_axis',(1.,0.,0.));
#9835=DIRECTION('center_axis',(0.,-1.,0.));
#9836=DIRECTION('ref_axis',(1.,0.,0.));
#9837=DIRECTION('center_axis',(0.,-1.,0.));
#9838=DIRECTION('ref_axis',(1.,0.,0.));
#9839=DIRECTION('',(0.707106781186548,0.707106781186547,8.65956056235493E-17));
#9840=DIRECTION('center_axis',(0.,-1.,0.));
#9841=DIRECTION('ref_axis',(1.,0.,0.));
#9842=DIRECTION('center_axis',(0.,-1.,0.));
#9843=DIRECTION('ref_axis',(1.,0.,0.));
#9844=DIRECTION('',(0.,1.,0.));
#9845=DIRECTION('center_axis',(0.,1.,0.));
#9846=DIRECTION('ref_axis',(1.,0.,0.));
#9847=DIRECTION('center_axis',(0.,-1.,0.));
#9848=DIRECTION('ref_axis',(1.,0.,0.));
#9849=DIRECTION('',(-0.707106781186547,0.707106781186548,-8.65956056235493E-17));
#9850=DIRECTION('center_axis',(0.,-1.,0.));
#9851=DIRECTION('ref_axis',(0.,0.,-1.));
#9852=DIRECTION('center_axis',(0.,-1.,0.));
#9853=DIRECTION('ref_axis',(1.,0.,0.));
#9854=DIRECTION('center_axis',(0.,1.,0.));
#9855=DIRECTION('ref_axis',(1.,0.,0.));
#9856=DIRECTION('center_axis',(0.,1.,0.));
#9857=DIRECTION('ref_axis',(1.,0.,0.));
#9858=DIRECTION('',(-0.447213595499958,0.894427190999916,-5.47678698264203E-17));
#9859=DIRECTION('center_axis',(0.,-1.,0.));
#9860=DIRECTION('ref_axis',(1.,0.,0.));
#9861=DIRECTION('center_axis',(0.,1.,0.));
#9862=DIRECTION('ref_axis',(1.,0.,0.));
#9863=DIRECTION('',(0.,1.,0.));
#9864=DIRECTION('center_axis',(0.,1.,0.));
#9865=DIRECTION('ref_axis',(1.,0.,0.));
#9866=DIRECTION('center_axis',(0.,-1.,0.));
#9867=DIRECTION('ref_axis',(1.,0.,0.));
#9868=DIRECTION('',(-0.707106781186547,0.707106781186548,-8.65956056235493E-17));
#9869=DIRECTION('center_axis',(0.,-1.,0.));
#9870=DIRECTION('ref_axis',(0.,0.,-1.));
#9871=DIRECTION('center_axis',(0.866025403784439,0.,-0.5));
#9872=DIRECTION('ref_axis',(0.5,0.,0.866025403784439));
#9873=DIRECTION('',(-0.5,0.,-0.866025403784439));
#9874=DIRECTION('',(0.,-1.,0.));
#9875=DIRECTION('',(0.5,0.,0.866025403784439));
#9876=DIRECTION('',(0.,-1.,0.));
#9877=DIRECTION('center_axis',(1.20185167898973E-16,0.,-1.));
#9878=DIRECTION('ref_axis',(1.,0.,1.20185167898973E-16));
#9879=DIRECTION('',(-1.,0.,-1.20185167898973E-16));
#9880=DIRECTION('',(0.,-1.,0.));
#9881=DIRECTION('',(1.,0.,1.20185167898973E-16));
#9882=DIRECTION('center_axis',(-0.866025403784439,0.,-0.5));
#9883=DIRECTION('ref_axis',(0.5,0.,-0.866025403784439));
#9884=DIRECTION('',(-0.5,0.,0.866025403784439));
#9885=DIRECTION('',(0.,-1.,0.));
#9886=DIRECTION('',(0.5,0.,-0.866025403784439));
#9887=DIRECTION('center_axis',(-0.866025403784439,0.,0.5));
#9888=DIRECTION('ref_axis',(-0.5,0.,-0.866025403784439));
#9889=DIRECTION('',(0.5,0.,0.866025403784439));
#9890=DIRECTION('',(0.,-1.,0.));
#9891=DIRECTION('',(-0.5,0.,-0.866025403784439));
#9892=DIRECTION('center_axis',(-2.40370335797945E-16,0.,1.));
#9893=DIRECTION('ref_axis',(-1.,0.,-2.40370335797945E-16));
#9894=DIRECTION('',(1.,0.,2.40370335797945E-16));
#9895=DIRECTION('',(0.,-1.,0.));
#9896=DIRECTION('',(-1.,0.,-2.40370335797945E-16));
#9897=DIRECTION('center_axis',(0.866025403784439,0.,0.5));
#9898=DIRECTION('ref_axis',(-0.5,0.,0.866025403784439));
#9899=DIRECTION('',(0.5,0.,-0.866025403784439));
#9900=DIRECTION('',(-0.5,0.,0.866025403784439));
#9901=DIRECTION('center_axis',(0.,1.,0.));
#9902=DIRECTION('ref_axis',(1.,0.,0.));
#9903=DIRECTION('center_axis',(0.,-1.,0.));
#9904=DIRECTION('ref_axis',(0.,0.,-1.));
#9905=DIRECTION('axis',(0.,0.,1.));
#9906=DIRECTION('refdir',(1.,0.,0.));
#9907=DIRECTION('center_axis',(0.,0.,1.));
#9908=DIRECTION('ref_axis',(1.,0.,0.));
#9909=DIRECTION('center_axis',(0.,0.,1.));
#9910=DIRECTION('ref_axis',(1.,0.,0.));
#9911=DIRECTION('',(0.,0.,1.));
#9912=DIRECTION('center_axis',(0.,0.,-1.));
#9913=DIRECTION('ref_axis',(1.,0.,0.));
#9914=DIRECTION('center_axis',(0.,0.,1.));
#9915=DIRECTION('ref_axis',(1.,0.,0.));
#9916=DIRECTION('center_axis',(0.,0.,1.));
#9917=DIRECTION('ref_axis',(1.,0.,0.));
#9918=DIRECTION('center_axis',(0.,0.,1.));
#9919=DIRECTION('ref_axis',(1.,0.,0.));
#9920=DIRECTION('center_axis',(0.,0.,1.));
#9921=DIRECTION('ref_axis',(1.,0.,0.));
#9922=DIRECTION('',(0.,0.,1.));
#9923=DIRECTION('center_axis',(0.,0.,-1.));
#9924=DIRECTION('ref_axis',(1.,0.,0.));
#9925=DIRECTION('center_axis',(0.,0.,1.));
#9926=DIRECTION('ref_axis',(1.,0.,0.));
#9927=DIRECTION('center_axis',(0.,0.,1.));
#9928=DIRECTION('ref_axis',(1.,0.,0.));
#9929=DIRECTION('center_axis',(0.,0.,1.));
#9930=DIRECTION('ref_axis',(1.,0.,0.));
#9931=DIRECTION('center_axis',(0.,0.,1.));
#9932=DIRECTION('ref_axis',(1.,0.,0.));
#9933=DIRECTION('',(0.,0.,1.));
#9934=DIRECTION('center_axis',(0.,0.,-1.));
#9935=DIRECTION('ref_axis',(1.,0.,0.));
#9936=DIRECTION('center_axis',(0.,0.,1.));
#9937=DIRECTION('ref_axis',(1.,0.,0.));
#9938=DIRECTION('center_axis',(0.,0.,1.));
#9939=DIRECTION('ref_axis',(1.,0.,0.));
#9940=DIRECTION('center_axis',(0.,0.,1.));
#9941=DIRECTION('ref_axis',(1.,0.,0.));
#9942=DIRECTION('center_axis',(0.,0.,1.));
#9943=DIRECTION('ref_axis',(1.,0.,0.));
#9944=DIRECTION('',(0.,0.,1.));
#9945=DIRECTION('center_axis',(0.,0.,-1.));
#9946=DIRECTION('ref_axis',(1.,0.,0.));
#9947=DIRECTION('center_axis',(0.,0.,1.));
#9948=DIRECTION('ref_axis',(1.,0.,0.));
#9949=DIRECTION('center_axis',(0.,0.,1.));
#9950=DIRECTION('ref_axis',(1.,0.,0.));
#9951=DIRECTION('center_axis',(0.,0.,1.));
#9952=DIRECTION('ref_axis',(1.,0.,0.));
#9953=DIRECTION('center_axis',(0.,0.,1.));
#9954=DIRECTION('ref_axis',(1.,0.,0.));
#9955=DIRECTION('',(0.,0.,1.));
#9956=DIRECTION('center_axis',(0.,0.,1.));
#9957=DIRECTION('ref_axis',(1.,0.,0.));
#9958=DIRECTION('center_axis',(0.,0.,1.));
#9959=DIRECTION('ref_axis',(1.,0.,0.));
#9960=DIRECTION('',(0.,0.,1.));
#9961=DIRECTION('center_axis',(0.,0.,1.));
#9962=DIRECTION('ref_axis',(1.,0.,0.));
#9963=DIRECTION('center_axis',(0.,0.,1.));
#9964=DIRECTION('ref_axis',(1.,0.,0.));
#9965=DIRECTION('',(0.,0.,1.));
#9966=DIRECTION('center_axis',(0.,0.,1.));
#9967=DIRECTION('ref_axis',(1.,0.,0.));
#9968=DIRECTION('center_axis',(0.,0.,1.));
#9969=DIRECTION('ref_axis',(1.,0.,0.));
#9970=DIRECTION('',(0.,0.,1.));
#9971=DIRECTION('center_axis',(0.,-0.56333682464151,0.826227342807548));
#9972=DIRECTION('ref_axis',(0.,-0.826227342807548,-0.56333682464151));
#9973=DIRECTION('',(0.,-0.826227342807548,-0.56333682464151));
#9974=DIRECTION('',(1.,0.,0.));
#9975=DIRECTION('',(0.,-0.826227342807548,-0.56333682464151));
#9976=DIRECTION('',(1.,0.,0.));
#9977=DIRECTION('center_axis',(0.,-1.,0.));
#9978=DIRECTION('ref_axis',(0.,0.,-1.));
#9979=DIRECTION('',(0.,0.,-1.));
#9980=DIRECTION('',(0.,0.,-1.));
#9981=DIRECTION('',(1.,0.,0.));
#9982=DIRECTION('center_axis',(0.,-0.56333682464151,-0.826227342807548));
#9983=DIRECTION('ref_axis',(0.,0.826227342807548,-0.56333682464151));
#9984=DIRECTION('',(0.,0.826227342807548,-0.56333682464151));
#9985=DIRECTION('',(0.,0.826227342807548,-0.56333682464151));
#9986=DIRECTION('',(1.,0.,0.));
#9987=DIRECTION('center_axis',(0.,-1.,0.));
#9988=DIRECTION('ref_axis',(0.,0.,-1.));
#9989=DIRECTION('',(0.,0.,-1.));
#9990=DIRECTION('',(0.,0.,-1.));
#9991=DIRECTION('',(1.,0.,0.));
#9992=DIRECTION('center_axis',(0.,0.,1.));
#9993=DIRECTION('ref_axis',(0.,-1.,0.));
#9994=DIRECTION('',(0.,-1.,0.));
#9995=DIRECTION('',(0.,-1.,0.));
#9996=DIRECTION('',(1.,0.,0.));
#9997=DIRECTION('center_axis',(0.,1.,0.));
#9998=DIRECTION('ref_axis',(0.,0.,1.));
#9999=DIRECTION('',(0.,0.,1.));
#10000=DIRECTION('',(0.,0.,1.));
#10001=DIRECTION('',(1.,0.,0.));
#10002=DIRECTION('center_axis',(0.,0.56333682464151,-0.826227342807548));
#10003=DIRECTION('ref_axis',(0.,0.826227342807548,0.56333682464151));
#10004=DIRECTION('',(0.,0.826227342807548,0.56333682464151));
#10005=DIRECTION('',(0.,0.826227342807548,0.56333682464151));
#10006=DIRECTION('',(1.,0.,0.));
#10007=DIRECTION('center_axis',(0.,1.,0.));
#10008=DIRECTION('ref_axis',(0.,0.,1.));
#10009=DIRECTION('',(0.,0.,1.));
#10010=DIRECTION('',(0.,0.,1.));
#10011=DIRECTION('',(1.,0.,0.));
#10012=DIRECTION('center_axis',(0.,0.56333682464151,0.826227342807548));
#10013=DIRECTION('ref_axis',(0.,-0.826227342807548,0.56333682464151));
#10014=DIRECTION('',(0.,-0.826227342807548,0.56333682464151));
#10015=DIRECTION('',(0.,-0.826227342807548,0.56333682464151));
#10016=DIRECTION('',(1.,0.,0.));
#10017=DIRECTION('center_axis',(0.,1.,0.));
#10018=DIRECTION('ref_axis',(0.,0.,1.));
#10019=DIRECTION('',(0.,0.,1.));
#10020=DIRECTION('',(0.,0.,1.));
#10021=DIRECTION('',(1.,0.,0.));
#10022=DIRECTION('center_axis',(0.,0.,-1.));
#10023=DIRECTION('ref_axis',(0.,1.,0.));
#10024=DIRECTION('',(0.,1.,0.));
#10025=DIRECTION('',(0.,1.,0.));
#10026=DIRECTION('',(1.,0.,0.));
#10027=DIRECTION('center_axis',(0.,-1.,0.));
#10028=DIRECTION('ref_axis',(0.,0.,-1.));
#10029=DIRECTION('',(0.,0.,-1.));
#10030=DIRECTION('',(0.,0.,-1.));
#10031=DIRECTION('center_axis',(1.,0.,0.));
#10032=DIRECTION('ref_axis',(0.,0.,-1.));
#10033=DIRECTION('center_axis',(1.,0.,0.));
#10034=DIRECTION('ref_axis',(0.,0.,-1.));
#10035=DIRECTION('axis',(0.,0.,1.));
#10036=DIRECTION('refdir',(1.,0.,0.));
#10037=DIRECTION('center_axis',(0.,0.,1.));
#10038=DIRECTION('ref_axis',(1.,0.,0.));
#10039=DIRECTION('',(1.,0.,0.));
#10040=DIRECTION('',(0.,-1.,0.));
#10041=DIRECTION('',(-1.,0.,0.));
#10042=DIRECTION('',(0.,1.,0.));
#10043=DIRECTION('center_axis',(0.,1.,0.));
#10044=DIRECTION('ref_axis',(-1.,0.,0.));
#10045=DIRECTION('',(0.,0.,1.));
#10046=DIRECTION('',(-1.,0.,0.));
#10047=DIRECTION('',(0.,0.,1.));
#10048=DIRECTION('center_axis',(0.,0.,1.));
#10049=DIRECTION('ref_axis',(1.,0.,0.));
#10050=DIRECTION('',(0.,-1.,0.));
#10051=DIRECTION('',(1.,0.,0.));
#10052=DIRECTION('',(0.,1.,0.));
#10053=DIRECTION('center_axis',(0.,0.,-1.));
#10054=DIRECTION('ref_axis',(1.,0.,0.));
#10055=DIRECTION('center_axis',(-1.,0.,0.));
#10056=DIRECTION('ref_axis',(0.,-1.,0.));
#10057=DIRECTION('',(0.,0.,1.));
#10058=DIRECTION('',(0.,0.707106781186548,0.707106781186548));
#10059=DIRECTION('',(0.,-1.,0.));
#10060=DIRECTION('',(0.,0.707106781186548,-0.707106781186548));
#10061=DIRECTION('',(0.,0.,1.));
#10062=DIRECTION('',(0.,-1.,0.));
#10063=DIRECTION('',(0.,0.,1.));
#10064=DIRECTION('center_axis',(0.,-1.,0.));
#10065=DIRECTION('ref_axis',(1.,0.,0.));
#10066=DIRECTION('',(1.,0.,0.));
#10067=DIRECTION('',(0.,0.,1.));
#10068=DIRECTION('center_axis',(0.,0.,1.));
#10069=DIRECTION('ref_axis',(1.,0.,0.));
#10070=DIRECTION('',(-1.,0.,0.));
#10071=DIRECTION('',(0.,1.,0.));
#10072=DIRECTION('center_axis',(1.,0.,0.));
#10073=DIRECTION('ref_axis',(0.,1.,0.));
#10074=DIRECTION('',(0.,0.,1.));
#10075=DIRECTION('',(0.,-0.707106781186548,0.707106781186548));
#10076=DIRECTION('',(0.,1.,0.));
#10077=DIRECTION('',(0.,-0.707106781186548,-0.707106781186548));
#10078=DIRECTION('',(0.,0.,1.));
#10079=DIRECTION('center_axis',(0.,-1.,0.));
#10080=DIRECTION('ref_axis',(1.,0.,0.));
#10081=DIRECTION('',(-1.,0.,0.));
#10082=DIRECTION('center_axis',(0.,-0.707106781186548,-0.707106781186548));
#10083=DIRECTION('ref_axis',(-1.,0.,0.));
#10084=DIRECTION('',(1.,0.,0.));
#10085=DIRECTION('center_axis',(0.,0.707106781186548,0.707106781186548));
#10086=DIRECTION('ref_axis',(0.,0.707106781186547,-0.707106781186547));
#10087=DIRECTION('',(1.,0.,0.));
#10088=DIRECTION('center_axis',(0.,0.,1.));
#10089=DIRECTION('ref_axis',(1.,0.,0.));
#10090=DIRECTION('center_axis',(0.,0.,-1.));
#10091=DIRECTION('ref_axis',(1.,0.,0.));
#10092=DIRECTION('',(0.,0.,1.));
#10093=DIRECTION('center_axis',(0.,0.,-1.));
#10094=DIRECTION('ref_axis',(1.,0.,0.));
#10095=DIRECTION('center_axis',(0.,-0.707106781186548,0.707106781186548));
#10096=DIRECTION('ref_axis',(0.,0.707106781186547,0.707106781186547));
#10097=DIRECTION('center_axis',(0.,0.,-1.));
#10098=DIRECTION('ref_axis',(1.,0.,0.));
#10099=DIRECTION('center_axis',(0.,0.,1.));
#10100=DIRECTION('ref_axis',(1.,0.,0.));
#10101=DIRECTION('',(-1.,0.,0.));
#10102=DIRECTION('center_axis',(0.,0.,1.));
#10103=DIRECTION('ref_axis',(1.,0.,0.));
#10104=DIRECTION('',(-1.,0.,0.));
#10105=DIRECTION('center_axis',(0.,0.707106781186548,-0.707106781186548));
#10106=DIRECTION('ref_axis',(-1.,0.,0.));
#10107=DIRECTION('',(1.,0.,0.));
#10108=DIRECTION('center_axis',(0.,1.,0.));
#10109=DIRECTION('ref_axis',(-1.,0.,0.));
#10110=DIRECTION('axis',(0.,0.,1.));
#10111=DIRECTION('refdir',(1.,0.,0.));
#10112=DIRECTION('center_axis',(0.,1.,0.));
#10113=DIRECTION('ref_axis',(1.,0.,0.));
#10114=DIRECTION('center_axis',(0.,1.,0.));
#10115=DIRECTION('ref_axis',(1.,0.,0.));
#10116=DIRECTION('',(0.707106781186548,-0.707106781186547,-8.65956056235494E-17));
#10117=DIRECTION('center_axis',(0.,-1.,0.));
#10118=DIRECTION('ref_axis',(1.,0.,0.));
#10119=DIRECTION('center_axis',(0.,1.,0.));
#10120=DIRECTION('ref_axis',(1.,0.,0.));
#10121=DIRECTION('',(0.,-1.,0.));
#10122=DIRECTION('center_axis',(0.,-1.,0.));
#10123=DIRECTION('ref_axis',(1.,0.,0.));
#10124=DIRECTION('center_axis',(0.,1.,0.));
#10125=DIRECTION('ref_axis',(1.,0.,0.));
#10126=DIRECTION('center_axis',(0.,1.,0.));
#10127=DIRECTION('ref_axis',(1.,0.,0.));
#10128=DIRECTION('center_axis',(0.,1.,0.));
#10129=DIRECTION('ref_axis',(1.,0.,0.));
#10130=DIRECTION('',(0.,-1.,0.));
#10131=DIRECTION('center_axis',(0.,1.,0.));
#10132=DIRECTION('ref_axis',(1.,0.,0.));
#10133=DIRECTION('center_axis',(0.,1.,0.));
#10134=DIRECTION('ref_axis',(1.,0.,0.));
#10135=DIRECTION('axis',(0.,0.,1.));
#10136=DIRECTION('refdir',(1.,0.,0.));
#10137=DIRECTION('center_axis',(0.866025403784439,0.,-0.5));
#10138=DIRECTION('ref_axis',(0.5,0.,0.866025403784439));
#10139=DIRECTION('',(-0.5,0.,-0.866025403784439));
#10140=DIRECTION('',(0.,-1.,0.));
#10141=DIRECTION('',(0.5,0.,0.866025403784439));
#10142=DIRECTION('',(0.,-1.,0.));
#10143=DIRECTION('center_axis',(1.20185167898973E-16,0.,-1.));
#10144=DIRECTION('ref_axis',(1.,0.,1.20185167898973E-16));
#10145=DIRECTION('',(-1.,0.,-1.20185167898973E-16));
#10146=DIRECTION('',(0.,-1.,0.));
#10147=DIRECTION('',(1.,0.,1.20185167898973E-16));
#10148=DIRECTION('center_axis',(-0.866025403784439,0.,-0.5));
#10149=DIRECTION('ref_axis',(0.5,0.,-0.866025403784439));
#10150=DIRECTION('',(-0.5,0.,0.866025403784439));
#10151=DIRECTION('',(0.,-1.,0.));
#10152=DIRECTION('',(0.5,0.,-0.866025403784439));
#10153=DIRECTION('center_axis',(-0.866025403784439,0.,0.5));
#10154=DIRECTION('ref_axis',(-0.5,0.,-0.866025403784439));
#10155=DIRECTION('',(0.5,0.,0.866025403784439));
#10156=DIRECTION('',(0.,-1.,0.));
#10157=DIRECTION('',(-0.5,0.,-0.866025403784439));
#10158=DIRECTION('center_axis',(-2.40370335797945E-16,0.,1.));
#10159=DIRECTION('ref_axis',(-1.,0.,-2.40370335797945E-16));
#10160=DIRECTION('',(1.,0.,2.40370335797945E-16));
#10161=DIRECTION('',(0.,-1.,0.));
#10162=DIRECTION('',(-1.,0.,-2.40370335797945E-16));
#10163=DIRECTION('center_axis',(0.866025403784439,0.,0.5));
#10164=DIRECTION('ref_axis',(-0.5,0.,0.866025403784439));
#10165=DIRECTION('',(0.5,0.,-0.866025403784439));
#10166=DIRECTION('',(-0.5,0.,0.866025403784439));
#10167=DIRECTION('center_axis',(0.,1.,0.));
#10168=DIRECTION('ref_axis',(1.,0.,0.));
#10169=DIRECTION('center_axis',(0.,-1.,0.));
#10170=DIRECTION('ref_axis',(0.,0.,-1.));
#10171=DIRECTION('center_axis',(0.,1.,0.));
#10172=DIRECTION('ref_axis',(1.,0.,0.));
#10173=DIRECTION('center_axis',(0.,1.,0.));
#10174=DIRECTION('ref_axis',(1.,0.,0.));
#10175=DIRECTION('center_axis',(0.,1.,0.));
#10176=DIRECTION('ref_axis',(1.,0.,0.));
#10177=DIRECTION('center_axis',(0.,1.,0.));
#10178=DIRECTION('ref_axis',(1.,0.,0.));
#10179=DIRECTION('',(0.,-1.,0.));
#10180=DIRECTION('center_axis',(0.,1.,0.));
#10181=DIRECTION('ref_axis',(1.,0.,0.));
#10182=DIRECTION('center_axis',(0.,1.,0.));
#10183=DIRECTION('ref_axis',(1.,0.,0.));
#10184=DIRECTION('center_axis',(0.,1.,0.));
#10185=DIRECTION('ref_axis',(0.,0.,1.));
#10186=DIRECTION('center_axis',(0.,-1.,0.));
#10187=DIRECTION('ref_axis',(1.,0.,0.));
#10188=DIRECTION('center_axis',(0.,-1.,0.));
#10189=DIRECTION('ref_axis',(1.,0.,0.));
#10190=DIRECTION('center_axis',(0.,-1.,0.));
#10191=DIRECTION('ref_axis',(1.,0.,0.));
#10192=DIRECTION('',(0.707106781186548,0.707106781186547,8.65956056235493E-17));
#10193=DIRECTION('center_axis',(0.,-1.,0.));
#10194=DIRECTION('ref_axis',(1.,0.,0.));
#10195=DIRECTION('center_axis',(0.,-1.,0.));
#10196=DIRECTION('ref_axis',(1.,0.,0.));
#10197=DIRECTION('',(0.,1.,0.));
#10198=DIRECTION('center_axis',(0.,1.,0.));
#10199=DIRECTION('ref_axis',(1.,0.,0.));
#10200=DIRECTION('center_axis',(0.,-1.,0.));
#10201=DIRECTION('ref_axis',(1.,0.,0.));
#10202=DIRECTION('',(-0.707106781186547,0.707106781186548,-8.65956056235493E-17));
#10203=DIRECTION('center_axis',(0.,-1.,0.));
#10204=DIRECTION('ref_axis',(0.,0.,-1.));
#10205=DIRECTION('center_axis',(0.,-1.,0.));
#10206=DIRECTION('ref_axis',(1.,0.,0.));
#10207=DIRECTION('center_axis',(0.,1.,0.));
#10208=DIRECTION('ref_axis',(1.,0.,0.));
#10209=DIRECTION('center_axis',(0.,1.,0.));
#10210=DIRECTION('ref_axis',(1.,0.,0.));
#10211=DIRECTION('',(-0.447213595499958,0.894427190999916,-5.47678698264203E-17));
#10212=DIRECTION('center_axis',(0.,-1.,0.));
#10213=DIRECTION('ref_axis',(1.,0.,0.));
#10214=DIRECTION('',(0.,1.,0.));
#10215=DIRECTION('axis',(0.,0.,1.));
#10216=DIRECTION('refdir',(1.,0.,0.));
#10217=DIRECTION('axis',(0.,0.,1.));
#10218=DIRECTION('refdir',(1.,0.,0.));
#10219=DIRECTION('center_axis',(1.,0.,0.));
#10220=DIRECTION('ref_axis',(0.,0.,-1.));
#10221=DIRECTION('center_axis',(1.,0.,0.));
#10222=DIRECTION('ref_axis',(0.,0.,-1.));
#10223=DIRECTION('',(1.,0.,0.));
#10224=DIRECTION('center_axis',(-1.,0.,0.));
#10225=DIRECTION('ref_axis',(0.,0.,-1.));
#10226=DIRECTION('center_axis',(1.,0.,0.));
#10227=DIRECTION('ref_axis',(0.,0.,-1.));
#10228=DIRECTION('center_axis',(1.,0.,0.));
#10229=DIRECTION('ref_axis',(0.,0.,-1.));
#10230=DIRECTION('',(1.,0.,0.));
#10231=DIRECTION('center_axis',(-1.,0.,0.));
#10232=DIRECTION('ref_axis',(0.,0.,-1.));
#10233=DIRECTION('center_axis',(1.,0.,0.));
#10234=DIRECTION('ref_axis',(0.,0.,-1.));
#10235=DIRECTION('center_axis',(1.,0.,0.));
#10236=DIRECTION('ref_axis',(0.,0.,-1.));
#10237=DIRECTION('',(1.,0.,0.));
#10238=DIRECTION('center_axis',(-1.,0.,0.));
#10239=DIRECTION('ref_axis',(0.,0.,-1.));
#10240=DIRECTION('center_axis',(1.,0.,0.));
#10241=DIRECTION('ref_axis',(0.,0.,-1.));
#10242=DIRECTION('center_axis',(1.,0.,0.));
#10243=DIRECTION('ref_axis',(0.,0.,-1.));
#10244=DIRECTION('',(1.,0.,0.));
#10245=DIRECTION('center_axis',(-1.,0.,0.));
#10246=DIRECTION('ref_axis',(0.,0.,-1.));
#10247=DIRECTION('center_axis',(1.,0.,0.));
#10248=DIRECTION('ref_axis',(0.,0.,-1.));
#10249=DIRECTION('center_axis',(1.,0.,0.));
#10250=DIRECTION('ref_axis',(0.,0.,-1.));
#10251=DIRECTION('',(1.,0.,0.));
#10252=DIRECTION('center_axis',(-1.,0.,0.));
#10253=DIRECTION('ref_axis',(0.,0.,-1.));
#10254=DIRECTION('center_axis',(1.,0.,0.));
#10255=DIRECTION('ref_axis',(0.,0.,-1.));
#10256=DIRECTION('center_axis',(1.,0.,0.));
#10257=DIRECTION('ref_axis',(0.,0.,-1.));
#10258=DIRECTION('',(1.,0.,0.));
#10259=DIRECTION('center_axis',(-1.,0.,0.));
#10260=DIRECTION('ref_axis',(0.,0.,-1.));
#10261=DIRECTION('center_axis',(0.,0.,1.));
#10262=DIRECTION('ref_axis',(0.,-1.,0.));
#10263=DIRECTION('',(-1.,0.,0.));
#10264=DIRECTION('',(0.,-1.,0.));
#10265=DIRECTION('',(1.,0.,0.));
#10266=DIRECTION('',(0.,-1.,0.));
#10267=DIRECTION('center_axis',(0.,0.,-1.));
#10268=DIRECTION('ref_axis',(0.,1.,0.));
#10269=DIRECTION('',(1.,0.,0.));
#10270=DIRECTION('',(0.,1.,0.));
#10271=DIRECTION('',(1.,0.,0.));
#10272=DIRECTION('',(0.,1.,0.));
#10273=DIRECTION('center_axis',(0.,1.,0.));
#10274=DIRECTION('ref_axis',(0.,0.,1.));
#10275=DIRECTION('',(0.,0.,1.));
#10276=DIRECTION('',(0.,0.,1.));
#10277=DIRECTION('center_axis',(1.,0.,0.));
#10278=DIRECTION('ref_axis',(0.,0.,-1.));
#10279=DIRECTION('',(0.,0.,1.));
#10280=DIRECTION('',(0.,1.,0.));
#10281=DIRECTION('',(0.,0.,-1.));
#10282=DIRECTION('',(0.,-1.,0.));
#10283=DIRECTION('',(0.,0.,1.));
#10284=DIRECTION('center_axis',(0.,1.,0.));
#10285=DIRECTION('ref_axis',(0.,0.,1.));
#10286=DIRECTION('',(0.,0.,1.));
#10287=DIRECTION('',(1.,0.,0.));
#10288=DIRECTION('center_axis',(0.,0.,1.));
#10289=DIRECTION('ref_axis',(0.,-1.,0.));
#10290=DIRECTION('',(1.,0.,0.));
#10291=DIRECTION('',(0.,-1.,0.));
#10292=DIRECTION('',(1.,0.,0.));
#10293=DIRECTION('center_axis',(0.,1.,0.));
#10294=DIRECTION('ref_axis',(0.,0.,1.));
#10295=DIRECTION('',(0.,0.,1.));
#10296=DIRECTION('center_axis',(0.,0.,-1.));
#10297=DIRECTION('ref_axis',(0.,1.,0.));
#10298=DIRECTION('',(0.,1.,0.));
#10299=DIRECTION('',(1.,0.,0.));
#10300=DIRECTION('center_axis',(0.,-1.,0.));
#10301=DIRECTION('ref_axis',(0.,0.,-1.));
#10302=DIRECTION('',(0.,0.,-1.));
#10303=DIRECTION('center_axis',(1.,0.,0.));
#10304=DIRECTION('ref_axis',(0.,0.,-1.));
#10305=DIRECTION('axis',(0.,0.,1.));
#10306=DIRECTION('refdir',(1.,0.,0.));
#10307=DIRECTION('center_axis',(1.,0.,0.));
#10308=DIRECTION('ref_axis',(0.,0.,-1.));
#10309=DIRECTION('center_axis',(1.,0.,0.));
#10310=DIRECTION('ref_axis',(0.,0.,-1.));
#10311=DIRECTION('',(1.,0.,0.));
#10312=DIRECTION('center_axis',(-1.,0.,0.));
#10313=DIRECTION('ref_axis',(0.,0.,-1.));
#10314=DIRECTION('center_axis',(1.,0.,0.));
#10315=DIRECTION('ref_axis',(0.,0.,-1.));
#10316=DIRECTION('center_axis',(1.,0.,0.));
#10317=DIRECTION('ref_axis',(0.,0.,-1.));
#10318=DIRECTION('center_axis',(1.,0.,0.));
#10319=DIRECTION('ref_axis',(0.,0.,-1.));
#10320=DIRECTION('',(1.,0.,0.));
#10321=DIRECTION('center_axis',(-1.,0.,0.));
#10322=DIRECTION('ref_axis',(0.,0.,-1.));
#10323=DIRECTION('center_axis',(1.,0.,0.));
#10324=DIRECTION('ref_axis',(0.,0.,-1.));
#10325=DIRECTION('center_axis',(1.,0.,0.));
#10326=DIRECTION('ref_axis',(0.,0.,-1.));
#10327=DIRECTION('center_axis',(1.,0.,0.));
#10328=DIRECTION('ref_axis',(0.,0.,-1.));
#10329=DIRECTION('',(-1.,0.,0.));
#10330=DIRECTION('center_axis',(-0.707106781186548,-0.707106781186548,0.));
#10331=DIRECTION('ref_axis',(-0.707106781186547,0.707106781186547,0.));
#10332=DIRECTION('center_axis',(1.,0.,0.));
#10333=DIRECTION('ref_axis',(0.,0.,-1.));
#10334=DIRECTION('center_axis',(1.,0.,0.));
#10335=DIRECTION('ref_axis',(0.,0.,-1.));
#10336=DIRECTION('center_axis',(1.,0.,0.));
#10337=DIRECTION('ref_axis',(0.,0.,-1.));
#10338=DIRECTION('',(0.,0.,-1.));
#10339=DIRECTION('center_axis',(0.,1.,0.));
#10340=DIRECTION('ref_axis',(1.,0.,0.));
#10341=DIRECTION('center_axis',(0.,1.,0.));
#10342=DIRECTION('ref_axis',(1.,0.,0.));
#10343=DIRECTION('center_axis',(0.,1.,0.));
#10344=DIRECTION('ref_axis',(1.,0.,0.));
#10345=DIRECTION('center_axis',(1.,0.,0.));
#10346=DIRECTION('ref_axis',(0.,0.,-1.));
#10347=DIRECTION('center_axis',(1.,0.,0.));
#10348=DIRECTION('ref_axis',(0.,0.,-1.));
#10349=DIRECTION('',(-1.,0.,0.));
#10350=DIRECTION('center_axis',(1.,0.,0.));
#10351=DIRECTION('ref_axis',(0.,0.,-1.));
#10352=DIRECTION('center_axis',(-0.707106781186548,0.707106781186548,0.));
#10353=DIRECTION('ref_axis',(0.707106781186547,0.707106781186547,0.));
#10354=DIRECTION('center_axis',(1.,0.,0.));
#10355=DIRECTION('ref_axis',(0.,0.,-1.));
#10356=DIRECTION('center_axis',(1.,0.,0.));
#10357=DIRECTION('ref_axis',(0.,0.,-1.));
#10358=DIRECTION('',(0.,0.,1.));
#10359=DIRECTION('center_axis',(0.,1.,0.));
#10360=DIRECTION('ref_axis',(1.,0.,0.));
#10361=DIRECTION('center_axis',(0.,1.,0.));
#10362=DIRECTION('ref_axis',(1.,0.,0.));
#10363=DIRECTION('center_axis',(0.,1.,0.));
#10364=DIRECTION('ref_axis',(1.,0.,0.));
#10365=DIRECTION('center_axis',(0.,1.,0.));
#10366=DIRECTION('ref_axis',(1.,0.,0.));
#10367=DIRECTION('',(0.,-1.,0.));
#10368=DIRECTION('axis',(0.,0.,1.));
#10369=DIRECTION('refdir',(1.,0.,0.));
#10370=DIRECTION('axis',(0.,0.,1.));
#10371=DIRECTION('refdir',(1.,0.,0.));
#10372=DIRECTION('center_axis',(0.,0.,1.));
#10373=DIRECTION('ref_axis',(1.,0.,0.));
#10374=DIRECTION('',(-1.,0.,0.));
#10375=DIRECTION('center_axis',(0.,0.,1.));
#10376=DIRECTION('ref_axis',(1.,0.,0.));
#10377=DIRECTION('center_axis',(0.,0.,1.));
#10378=DIRECTION('ref_axis',(1.,0.,0.));
#10379=DIRECTION('',(0.,0.,-1.));
#10380=DIRECTION('center_axis',(0.,0.,1.));
#10381=DIRECTION('ref_axis',(1.,0.,0.));
#10382=DIRECTION('',(0.,0.,1.));
#10383=DIRECTION('center_axis',(0.,0.,-1.));
#10384=DIRECTION('ref_axis',(1.,0.,0.));
#10385=DIRECTION('center_axis',(0.,0.,1.));
#10386=DIRECTION('ref_axis',(1.,0.,0.));
#10387=DIRECTION('',(0.,0.,1.));
#10388=DIRECTION('center_axis',(0.,0.,1.));
#10389=DIRECTION('ref_axis',(1.,0.,0.));
#10390=DIRECTION('',(1.,0.,0.));
#10391=DIRECTION('center_axis',(0.,0.,1.));
#10392=DIRECTION('ref_axis',(1.,0.,0.));
#10393=DIRECTION('center_axis',(0.,0.,1.));
#10394=DIRECTION('ref_axis',(1.,0.,0.));
#10395=DIRECTION('',(0.,0.,-1.));
#10396=DIRECTION('center_axis',(0.,0.,1.));
#10397=DIRECTION('ref_axis',(1.,0.,0.));
#10398=DIRECTION('',(0.,0.,1.));
#10399=DIRECTION('center_axis',(0.,0.,-1.));
#10400=DIRECTION('ref_axis',(1.,0.,0.));
#10401=DIRECTION('center_axis',(0.,0.,1.));
#10402=DIRECTION('ref_axis',(1.,0.,0.));
#10403=DIRECTION('',(0.,0.,1.));
#10404=DIRECTION('center_axis',(0.,0.,1.));
#10405=DIRECTION('ref_axis',(1.,0.,0.));
#10406=DIRECTION('',(-1.,0.,0.));
#10407=DIRECTION('center_axis',(0.,0.,1.));
#10408=DIRECTION('ref_axis',(1.,0.,0.));
#10409=DIRECTION('center_axis',(0.,0.,1.));
#10410=DIRECTION('ref_axis',(1.,0.,0.));
#10411=DIRECTION('',(0.,0.,-1.));
#10412=DIRECTION('center_axis',(0.,0.,1.));
#10413=DIRECTION('ref_axis',(1.,0.,0.));
#10414=DIRECTION('',(0.,0.,1.));
#10415=DIRECTION('center_axis',(0.,0.,-1.));
#10416=DIRECTION('ref_axis',(1.,0.,0.));
#10417=DIRECTION('center_axis',(0.,0.,1.));
#10418=DIRECTION('ref_axis',(1.,0.,0.));
#10419=DIRECTION('',(0.,0.,1.));
#10420=DIRECTION('center_axis',(0.,0.,1.));
#10421=DIRECTION('ref_axis',(1.,0.,0.));
#10422=DIRECTION('',(1.,0.,0.));
#10423=DIRECTION('center_axis',(0.,0.,1.));
#10424=DIRECTION('ref_axis',(1.,0.,0.));
#10425=DIRECTION('center_axis',(0.,0.,1.));
#10426=DIRECTION('ref_axis',(1.,0.,0.));
#10427=DIRECTION('',(0.,0.,-1.));
#10428=DIRECTION('center_axis',(0.,0.,1.));
#10429=DIRECTION('ref_axis',(1.,0.,0.));
#10430=DIRECTION('',(0.,0.,1.));
#10431=DIRECTION('center_axis',(0.,0.,-1.));
#10432=DIRECTION('ref_axis',(1.,0.,0.));
#10433=DIRECTION('center_axis',(0.,0.,1.));
#10434=DIRECTION('ref_axis',(1.,0.,0.));
#10435=DIRECTION('',(0.,0.,1.));
#10436=DIRECTION('center_axis',(0.,-1.,0.));
#10437=DIRECTION('ref_axis',(0.,0.,-1.));
#10438=DIRECTION('',(-1.,0.,0.));
#10439=DIRECTION('',(-1.,0.,0.));
#10440=DIRECTION('',(0.,0.,1.));
#10441=DIRECTION('',(1.,0.,0.));
#10442=DIRECTION('',(0.,0.,-1.));
#10443=DIRECTION('',(-1.,0.,0.));
#10444=DIRECTION('center_axis',(0.,1.,0.));
#10445=DIRECTION('ref_axis',(0.,0.,1.));
#10446=DIRECTION('',(1.,0.,0.));
#10447=DIRECTION('',(1.,0.,0.));
#10448=DIRECTION('',(0.,0.,1.));
#10449=DIRECTION('',(1.,0.,0.));
#10450=DIRECTION('',(0.,0.,-1.));
#10451=DIRECTION('',(1.,0.,0.));
#10452=DIRECTION('center_axis',(-1.,0.,0.));
#10453=DIRECTION('ref_axis',(0.,0.,1.));
#10454=DIRECTION('',(0.,-1.,0.));
#10455=DIRECTION('',(0.,0.,1.));
#10456=DIRECTION('',(0.,1.,0.));
#10457=DIRECTION('',(0.,0.,-1.));
#10458=DIRECTION('',(0.,-1.,0.));
#10459=DIRECTION('',(0.,-1.,0.));
#10460=DIRECTION('',(0.,0.,1.));
#10461=DIRECTION('',(0.,-1.,0.));
#10462=DIRECTION('',(0.,0.,-1.));
#10463=DIRECTION('',(0.,-1.,0.));
#10464=DIRECTION('center_axis',(0.,0.,-1.));
#10465=DIRECTION('ref_axis',(0.,1.,0.));
#10466=DIRECTION('',(0.,1.,0.));
#10467=DIRECTION('',(1.,0.,0.));
#10468=DIRECTION('center_axis',(0.,-1.,0.));
#10469=DIRECTION('ref_axis',(0.,0.,-1.));
#10470=DIRECTION('',(0.,0.,-1.));
#10471=DIRECTION('',(1.,0.,0.));
#10472=DIRECTION('center_axis',(0.,0.,1.));
#10473=DIRECTION('ref_axis',(0.,-1.,0.));
#10474=DIRECTION('',(0.,-1.,0.));
#10475=DIRECTION('',(1.,0.,0.));
#10476=DIRECTION('center_axis',(0.,1.,0.));
#10477=DIRECTION('ref_axis',(0.,0.,1.));
#10478=DIRECTION('',(0.,0.,1.));
#10479=DIRECTION('',(1.,0.,0.));
#10480=DIRECTION('center_axis',(0.,0.,-1.));
#10481=DIRECTION('ref_axis',(0.,1.,0.));
#10482=DIRECTION('',(0.,1.,0.));
#10483=DIRECTION('center_axis',(0.,0.,-1.));
#10484=DIRECTION('ref_axis',(0.,1.,0.));
#10485=DIRECTION('',(0.,1.,0.));
#10486=DIRECTION('',(1.,0.,0.));
#10487=DIRECTION('center_axis',(0.,-1.,0.));
#10488=DIRECTION('ref_axis',(0.,0.,-1.));
#10489=DIRECTION('',(0.,0.,-1.));
#10490=DIRECTION('',(1.,0.,0.));
#10491=DIRECTION('center_axis',(0.,0.,-1.));
#10492=DIRECTION('ref_axis',(0.,1.,0.));
#10493=DIRECTION('',(0.,1.,0.));
#10494=DIRECTION('',(1.,0.,0.));
#10495=DIRECTION('center_axis',(0.,1.,0.));
#10496=DIRECTION('ref_axis',(0.,0.,1.));
#10497=DIRECTION('',(0.,0.,1.));
#10498=DIRECTION('',(1.,0.,0.));
#10499=DIRECTION('center_axis',(0.,0.,-1.));
#10500=DIRECTION('ref_axis',(0.,1.,0.));
#10501=DIRECTION('',(0.,1.,0.));
#10502=DIRECTION('center_axis',(1.,0.,0.));
#10503=DIRECTION('ref_axis',(0.,0.,-1.));
#10504=DIRECTION('axis',(0.,0.,1.));
#10505=DIRECTION('refdir',(1.,0.,0.));
#10506=DIRECTION('center_axis',(0.,0.,1.));
#10507=DIRECTION('ref_axis',(0.,-1.,0.));
#10508=DIRECTION('',(0.,-1.,0.));
#10509=DIRECTION('',(1.,0.,0.));
#10510=DIRECTION('',(0.,-1.,0.));
#10511=DIRECTION('',(1.,0.,0.));
#10512=DIRECTION('center_axis',(0.,1.,0.));
#10513=DIRECTION('ref_axis',(0.,0.,1.));
#10514=DIRECTION('',(0.,0.,1.));
#10515=DIRECTION('',(0.,0.,1.));
#10516=DIRECTION('',(1.,0.,0.));
#10517=DIRECTION('center_axis',(0.,0.,-1.));
#10518=DIRECTION('ref_axis',(0.,1.,0.));
#10519=DIRECTION('',(0.,1.,0.));
#10520=DIRECTION('',(0.,1.,0.));
#10521=DIRECTION('',(1.,0.,0.));
#10522=DIRECTION('center_axis',(0.,-1.,0.));
#10523=DIRECTION('ref_axis',(0.,0.,-1.));
#10524=DIRECTION('',(0.,0.,-1.));
#10525=DIRECTION('',(0.,0.,-1.));
#10526=DIRECTION('',(1.,0.,0.));
#10527=DIRECTION('center_axis',(0.,0.,-1.));
#10528=DIRECTION('ref_axis',(0.,1.,0.));
#10529=DIRECTION('',(0.,1.,0.));
#10530=DIRECTION('',(0.,1.,0.));
#10531=DIRECTION('',(1.,0.,0.));
#10532=DIRECTION('center_axis',(0.,1.,0.));
#10533=DIRECTION('ref_axis',(0.,0.,1.));
#10534=DIRECTION('',(0.,0.,1.));
#10535=DIRECTION('',(0.,0.,1.));
#10536=DIRECTION('',(1.,0.,0.));
#10537=DIRECTION('center_axis',(0.,0.,-1.));
#10538=DIRECTION('ref_axis',(0.,1.,0.));
#10539=DIRECTION('',(0.,1.,0.));
#10540=DIRECTION('',(0.,1.,0.));
#10541=DIRECTION('',(1.,0.,0.));
#10542=DIRECTION('center_axis',(0.,-1.,0.));
#10543=DIRECTION('ref_axis',(0.,0.,-1.));
#10544=DIRECTION('',(0.,0.,-1.));
#10545=DIRECTION('',(0.,0.,-1.));
#10546=DIRECTION('center_axis',(1.,0.,0.));
#10547=DIRECTION('ref_axis',(0.,0.,-1.));
#10548=DIRECTION('center_axis',(1.,0.,0.));
#10549=DIRECTION('ref_axis',(0.,0.,-1.));
#10550=DIRECTION('axis',(0.,0.,1.));
#10551=DIRECTION('refdir',(1.,0.,0.));
#10552=DIRECTION('center_axis',(0.,0.,-1.));
#10553=DIRECTION('ref_axis',(0.,-1.,0.));
#10554=DIRECTION('',(0.,1.,0.));
#10555=DIRECTION('',(-1.,0.,0.));
#10556=DIRECTION('',(0.,-1.,0.));
#10557=DIRECTION('',(-1.,0.,0.));
#10558=DIRECTION('center_axis',(0.,1.,0.));
#10559=DIRECTION('ref_axis',(0.,0.,-1.));
#10560=DIRECTION('',(0.,0.,1.));
#10561=DIRECTION('',(0.,0.,-1.));
#10562=DIRECTION('',(-1.,0.,0.));
#10563=DIRECTION('center_axis',(0.,0.,-1.));
#10564=DIRECTION('ref_axis',(0.,-1.,0.));
#10565=DIRECTION('',(0.,1.,0.));
#10566=DIRECTION('',(0.,-1.,0.));
#10567=DIRECTION('',(-1.,0.,0.));
#10568=DIRECTION('center_axis',(0.,-1.,0.));
#10569=DIRECTION('ref_axis',(0.,0.,1.));
#10570=DIRECTION('',(0.,0.,-1.));
#10571=DIRECTION('',(0.,0.,1.));
#10572=DIRECTION('',(-1.,0.,0.));
#10573=DIRECTION('center_axis',(0.,0.,-1.));
#10574=DIRECTION('ref_axis',(0.,-1.,0.));
#10575=DIRECTION('',(0.,1.,0.));
#10576=DIRECTION('',(0.,-1.,0.));
#10577=DIRECTION('',(-1.,0.,0.));
#10578=DIRECTION('center_axis',(0.,1.,0.));
#10579=DIRECTION('ref_axis',(0.,0.,-1.));
#10580=DIRECTION('',(0.,0.,1.));
#10581=DIRECTION('',(0.,0.,-1.));
#10582=DIRECTION('',(-1.,0.,0.));
#10583=DIRECTION('center_axis',(0.,0.,1.));
#10584=DIRECTION('ref_axis',(0.,1.,0.));
#10585=DIRECTION('',(0.,-1.,0.));
#10586=DIRECTION('',(0.,1.,0.));
#10587=DIRECTION('',(-1.,0.,0.));
#10588=DIRECTION('center_axis',(0.,-1.,0.));
#10589=DIRECTION('ref_axis',(0.,0.,1.));
#10590=DIRECTION('',(0.,0.,-1.));
#10591=DIRECTION('',(0.,0.,1.));
#10592=DIRECTION('center_axis',(1.,0.,0.));
#10593=DIRECTION('ref_axis',(0.,0.,-1.));
#10594=DIRECTION('center_axis',(-1.,0.,0.));
#10595=DIRECTION('ref_axis',(0.,0.,1.));
#10596=DIRECTION('',(0.,0.,1.));
#10597=DIRECTION('',(1.,0.,0.));
#10598=DIRECTION('',(0.,0.,1.));
#10599=DIRECTION('',(1.,0.,0.));
#10600=DIRECTION('',(0.,0.,1.));
#10601=DIRECTION('',(1.,0.,0.));
#10602=DIRECTION('axis',(0.,0.,1.));
#10603=DIRECTION('refdir',(1.,0.,0.));
#10604=DIRECTION('center_axis',(0.866025403784439,0.,-0.5));
#10605=DIRECTION('ref_axis',(0.5,0.,0.866025403784439));
#10606=DIRECTION('',(-0.5,0.,-0.866025403784439));
#10607=DIRECTION('',(0.,-1.,0.));
#10608=DIRECTION('',(0.5,0.,0.866025403784439));
#10609=DIRECTION('',(0.,-1.,0.));
#10610=DIRECTION('center_axis',(1.20185167898973E-16,0.,-1.));
#10611=DIRECTION('ref_axis',(1.,0.,1.20185167898973E-16));
#10612=DIRECTION('',(-1.,0.,-1.20185167898973E-16));
#10613=DIRECTION('',(0.,-1.,0.));
#10614=DIRECTION('',(1.,0.,1.20185167898973E-16));
#10615=DIRECTION('center_axis',(-0.866025403784439,0.,-0.5));
#10616=DIRECTION('ref_axis',(0.5,0.,-0.866025403784439));
#10617=DIRECTION('',(-0.5,0.,0.866025403784439));
#10618=DIRECTION('',(0.,-1.,0.));
#10619=DIRECTION('',(0.5,0.,-0.866025403784439));
#10620=DIRECTION('center_axis',(-0.866025403784439,0.,0.5));
#10621=DIRECTION('ref_axis',(-0.5,0.,-0.866025403784439));
#10622=DIRECTION('',(0.5,0.,0.866025403784439));
#10623=DIRECTION('',(0.,-1.,0.));
#10624=DIRECTION('',(-0.5,0.,-0.866025403784439));
#10625=DIRECTION('center_axis',(-2.40370335797945E-16,0.,1.));
#10626=DIRECTION('ref_axis',(-1.,0.,-2.40370335797945E-16));
#10627=DIRECTION('',(1.,0.,2.40370335797945E-16));
#10628=DIRECTION('',(0.,-1.,0.));
#10629=DIRECTION('',(-1.,0.,-2.40370335797945E-16));
#10630=DIRECTION('center_axis',(0.866025403784439,0.,0.5));
#10631=DIRECTION('ref_axis',(-0.5,0.,0.866025403784439));
#10632=DIRECTION('',(0.5,0.,-0.866025403784439));
#10633=DIRECTION('',(-0.5,0.,0.866025403784439));
#10634=DIRECTION('center_axis',(0.,1.,0.));
#10635=DIRECTION('ref_axis',(1.,0.,0.));
#10636=DIRECTION('center_axis',(0.,-1.,0.));
#10637=DIRECTION('ref_axis',(0.,0.,-1.));
#10638=DIRECTION('center_axis',(0.,1.,0.));
#10639=DIRECTION('ref_axis',(1.,0.,0.));
#10640=DIRECTION('center_axis',(0.,1.,0.));
#10641=DIRECTION('ref_axis',(1.,0.,0.));
#10642=DIRECTION('center_axis',(0.,1.,0.));
#10643=DIRECTION('ref_axis',(0.,0.,1.));
#10644=DIRECTION('center_axis',(0.,-1.,0.));
#10645=DIRECTION('ref_axis',(1.,0.,0.));
#10646=DIRECTION('center_axis',(0.,-1.,0.));
#10647=DIRECTION('ref_axis',(1.,0.,0.));
#10648=DIRECTION('center_axis',(0.,-1.,0.));
#10649=DIRECTION('ref_axis',(1.,0.,0.));
#10650=DIRECTION('',(0.707106781186548,0.707106781186547,8.65956056235493E-17));
#10651=DIRECTION('center_axis',(0.,-1.,0.));
#10652=DIRECTION('ref_axis',(1.,0.,0.));
#10653=DIRECTION('center_axis',(0.,-1.,0.));
#10654=DIRECTION('ref_axis',(1.,0.,0.));
#10655=DIRECTION('',(0.,1.,0.));
#10656=DIRECTION('center_axis',(0.,1.,0.));
#10657=DIRECTION('ref_axis',(1.,0.,0.));
#10658=DIRECTION('center_axis',(0.,-1.,0.));
#10659=DIRECTION('ref_axis',(1.,0.,0.));
#10660=DIRECTION('',(-0.707106781186547,0.707106781186548,-8.65956056235493E-17));
#10661=DIRECTION('center_axis',(0.,-1.,0.));
#10662=DIRECTION('ref_axis',(0.,0.,-1.));
#10663=DIRECTION('center_axis',(0.,-1.,0.));
#10664=DIRECTION('ref_axis',(1.,0.,0.));
#10665=DIRECTION('center_axis',(0.,1.,0.));
#10666=DIRECTION('ref_axis',(1.,0.,0.));
#10667=DIRECTION('center_axis',(0.,1.,0.));
#10668=DIRECTION('ref_axis',(1.,0.,0.));
#10669=DIRECTION('',(-0.447213595499958,0.894427190999916,-5.47678698264203E-17));
#10670=DIRECTION('center_axis',(0.,-1.,0.));
#10671=DIRECTION('ref_axis',(1.,0.,0.));
#10672=DIRECTION('',(0.,1.,0.));
#10673=DIRECTION('axis',(0.,0.,1.));
#10674=DIRECTION('refdir',(1.,0.,0.));
#10675=DIRECTION('center_axis',(0.,1.,0.));
#10676=DIRECTION('ref_axis',(0.,0.,1.));
#10677=DIRECTION('center_axis',(0.,-1.,0.));
#10678=DIRECTION('ref_axis',(1.,0.,0.));
#10679=DIRECTION('center_axis',(0.,-1.,0.));
#10680=DIRECTION('ref_axis',(1.,0.,0.));
#10681=DIRECTION('center_axis',(0.,-1.,0.));
#10682=DIRECTION('ref_axis',(1.,0.,0.));
#10683=DIRECTION('',(0.707106781186547,0.707106781186548,8.65956056235493E-17));
#10684=DIRECTION('center_axis',(0.,-1.,0.));
#10685=DIRECTION('ref_axis',(1.,0.,0.));
#10686=DIRECTION('center_axis',(0.,-1.,0.));
#10687=DIRECTION('ref_axis',(1.,0.,0.));
#10688=DIRECTION('',(0.,1.,0.));
#10689=DIRECTION('center_axis',(0.,1.,0.));
#10690=DIRECTION('ref_axis',(1.,0.,0.));
#10691=DIRECTION('center_axis',(0.,-1.,0.));
#10692=DIRECTION('ref_axis',(1.,0.,0.));
#10693=DIRECTION('',(-0.707106781186547,0.707106781186548,-8.65956056235493E-17));
#10694=DIRECTION('center_axis',(0.,-1.,0.));
#10695=DIRECTION('ref_axis',(0.,0.,-1.));
#10696=DIRECTION('center_axis',(0.,-1.,0.));
#10697=DIRECTION('ref_axis',(1.,0.,0.));
#10698=DIRECTION('center_axis',(0.,1.,0.));
#10699=DIRECTION('ref_axis',(1.,0.,0.));
#10700=DIRECTION('center_axis',(0.,1.,0.));
#10701=DIRECTION('ref_axis',(1.,0.,0.));
#10702=DIRECTION('',(-0.447213595499958,0.894427190999916,-5.47678698264203E-17));
#10703=DIRECTION('center_axis',(0.,-1.,0.));
#10704=DIRECTION('ref_axis',(1.,0.,0.));
#10705=DIRECTION('center_axis',(0.,1.,0.));
#10706=DIRECTION('ref_axis',(1.,0.,0.));
#10707=DIRECTION('',(0.,1.,0.));
#10708=DIRECTION('center_axis',(0.,1.,0.));
#10709=DIRECTION('ref_axis',(1.,0.,0.));
#10710=DIRECTION('center_axis',(0.,-1.,0.));
#10711=DIRECTION('ref_axis',(1.,0.,0.));
#10712=DIRECTION('',(-0.707106781186547,0.707106781186548,-8.65956056235493E-17));
#10713=DIRECTION('center_axis',(0.,-1.,0.));
#10714=DIRECTION('ref_axis',(0.,0.,-1.));
#10715=DIRECTION('center_axis',(0.866025403784439,0.,-0.5));
#10716=DIRECTION('ref_axis',(0.5,0.,0.866025403784439));
#10717=DIRECTION('',(-0.5,0.,-0.866025403784439));
#10718=DIRECTION('',(0.,-1.,0.));
#10719=DIRECTION('',(0.5,0.,0.866025403784439));
#10720=DIRECTION('',(0.,-1.,0.));
#10721=DIRECTION('center_axis',(1.60246890531964E-16,0.,-1.));
#10722=DIRECTION('ref_axis',(1.,0.,1.60246890531964E-16));
#10723=DIRECTION('',(-1.,0.,-1.60246890531964E-16));
#10724=DIRECTION('',(0.,-1.,0.));
#10725=DIRECTION('',(1.,0.,1.60246890531964E-16));
#10726=DIRECTION('center_axis',(-0.866025403784439,0.,-0.5));
#10727=DIRECTION('ref_axis',(0.5,0.,-0.866025403784439));
#10728=DIRECTION('',(-0.5,0.,0.866025403784439));
#10729=DIRECTION('',(0.,-1.,0.));
#10730=DIRECTION('',(0.5,0.,-0.866025403784439));
#10731=DIRECTION('center_axis',(-0.866025403784439,0.,0.5));
#10732=DIRECTION('ref_axis',(-0.5,0.,-0.866025403784439));
#10733=DIRECTION('',(0.5,0.,0.866025403784439));
#10734=DIRECTION('',(0.,-1.,0.));
#10735=DIRECTION('',(-0.5,0.,-0.866025403784439));
#10736=DIRECTION('center_axis',(-1.60246890531964E-16,0.,1.));
#10737=DIRECTION('ref_axis',(-1.,0.,-1.60246890531964E-16));
#10738=DIRECTION('',(1.,0.,1.60246890531964E-16));
#10739=DIRECTION('',(0.,-1.,0.));
#10740=DIRECTION('',(-1.,0.,-1.60246890531964E-16));
#10741=DIRECTION('center_axis',(0.866025403784439,0.,0.5));
#10742=DIRECTION('ref_axis',(-0.5,0.,0.866025403784439));
#10743=DIRECTION('',(0.5,0.,-0.866025403784439));
#10744=DIRECTION('',(-0.5,0.,0.866025403784439));
#10745=DIRECTION('center_axis',(0.,1.,0.));
#10746=DIRECTION('ref_axis',(1.,0.,0.));
#10747=DIRECTION('center_axis',(0.,-1.,0.));
#10748=DIRECTION('ref_axis',(0.,0.,-1.));
#10749=DIRECTION('',(0.,0.,1.));
#10750=DIRECTION('',(1.,0.,0.));
#10751=DIRECTION('',(0.,0.,1.));
#10752=DIRECTION('',(1.,0.,0.));
#10753=DIRECTION('',(0.,0.,1.));
#10754=DIRECTION('',(1.,0.,0.));
#10755=DIRECTION('',(0.,0.,1.));
#10756=DIRECTION('',(1.,0.,0.));
#10757=DIRECTION('',(0.,0.,1.));
#10758=DIRECTION('',(1.,0.,0.));
#10759=DIRECTION('',(0.,0.,1.));
#10760=DIRECTION('',(1.,0.,0.));
#10761=DIRECTION('',(0.,0.,1.));
#10762=DIRECTION('',(1.,0.,0.));
#10763=DIRECTION('',(0.,0.,1.));
#10764=DIRECTION('',(1.,0.,0.));
#10765=DIRECTION('',(0.,0.,1.));
#10766=DIRECTION('',(1.,0.,0.));
#10767=DIRECTION('',(0.,0.,1.));
#10768=DIRECTION('',(1.,0.,0.));
#10769=DIRECTION('',(0.,0.,1.));
#10770=DIRECTION('',(1.,0.,0.));
#10771=DIRECTION('',(0.,0.,1.));
#10772=DIRECTION('',(1.,0.,0.));
#10773=DIRECTION('',(0.,0.,1.));
#10774=DIRECTION('',(1.,0.,0.));
#10775=DIRECTION('',(0.,0.,1.));
#10776=DIRECTION('',(1.,0.,0.));
#10777=DIRECTION('',(0.,0.,1.));
#10778=DIRECTION('',(1.,0.,0.));
#10779=DIRECTION('',(0.,0.,1.));
#10780=DIRECTION('',(1.,0.,0.));
#10781=DIRECTION('',(0.,0.,1.));
#10782=DIRECTION('',(1.,0.,0.));
#10783=DIRECTION('',(0.,0.,1.));
#10784=DIRECTION('',(1.,0.,0.));
#10785=DIRECTION('',(0.,0.,1.));
#10786=DIRECTION('',(1.,0.,0.));
#10787=DIRECTION('',(-1.,0.,2.22044604925031E-16));
#10788=DIRECTION('',(2.22044604925031E-16,0.,1.));
#10789=DIRECTION('',(0.,1.,2.22044604925031E-16));
#10790=DIRECTION('',(1.,0.,0.));
#10791=DIRECTION('',(0.,-1.,2.22044604925031E-16));
#10792=DIRECTION('',(1.,0.,0.));
#10793=DIRECTION('',(-1.,0.,2.22044604925031E-16));
#10794=DIRECTION('',(2.22044604925031E-16,0.,1.));
#10795=DIRECTION('',(0.,1.,2.22044604925031E-16));
#10796=DIRECTION('',(1.,0.,0.));
#10797=DIRECTION('',(0.,-1.,2.22044604925031E-16));
#10798=DIRECTION('',(1.,0.,0.));
#10799=DIRECTION('',(-1.,0.,2.22044604925031E-16));
#10800=DIRECTION('',(2.22044604925031E-16,0.,1.));
#10801=DIRECTION('',(0.,1.,2.22044604925031E-16));
#10802=DIRECTION('',(1.,0.,0.));
#10803=DIRECTION('',(0.,-1.,2.22044604925031E-16));
#10804=DIRECTION('',(1.,0.,0.));
#10805=DIRECTION('',(-1.,0.,2.22044604925031E-16));
#10806=DIRECTION('',(2.22044604925031E-16,0.,1.));
#10807=DIRECTION('',(0.,1.,2.22044604925031E-16));
#10808=DIRECTION('',(1.,0.,0.));
#10809=DIRECTION('',(0.,-1.,2.22044604925031E-16));
#10810=DIRECTION('',(1.,0.,0.));
#10811=DIRECTION('',(0.,1.,0.));
#10812=DIRECTION('',(0.,0.,1.));
#10813=DIRECTION('',(0.,0.,1.));
#10814=DIRECTION('',(1.,0.,0.));
#10815=DIRECTION('',(0.,0.,1.));
#10816=DIRECTION('',(1.,0.,0.));
#10817=DIRECTION('',(0.,-1.,0.));
#10818=DIRECTION('',(0.,0.,-1.));
#10819=DIRECTION('',(0.,0.,1.));
#10820=DIRECTION('',(-1.,1.22464679914735E-16,0.));
#10821=DIRECTION('',(0.,0.,1.));
#10822=DIRECTION('',(-1.,1.22464679914735E-16,0.));
#10823=DIRECTION('',(0.,1.,0.));
#10824=DIRECTION('',(0.,0.,1.));
#10825=DIRECTION('',(0.,0.,1.));
#10826=DIRECTION('',(1.,0.,0.));
#10827=DIRECTION('',(0.,0.,1.));
#10828=DIRECTION('',(1.,0.,0.));
#10829=DIRECTION('',(0.,-1.,0.));
#10830=DIRECTION('',(0.,0.,-1.));
#10831=DIRECTION('',(0.,0.,1.));
#10832=DIRECTION('',(-1.,1.22464679914735E-16,0.));
#10833=DIRECTION('',(0.,0.,1.));
#10834=DIRECTION('',(-1.,1.22464679914735E-16,0.));
#10835=DIRECTION('',(-1.,0.,2.22044604925031E-16));
#10836=DIRECTION('',(2.22044604925031E-16,0.,1.));
#10837=DIRECTION('',(0.,0.,1.));
#10838=DIRECTION('',(2.22044604925031E-16,1.,0.));
#10839=DIRECTION('',(0.,0.,1.));
#10840=DIRECTION('',(2.22044604925031E-16,1.,0.));
#10841=DIRECTION('',(-1.,0.,2.22044604925031E-16));
#10842=DIRECTION('',(2.22044604925031E-16,0.,1.));
#10843=DIRECTION('',(0.,0.,1.));
#10844=DIRECTION('',(2.22044604925031E-16,1.,0.));
#10845=DIRECTION('',(0.,0.,1.));
#10846=DIRECTION('',(2.22044604925031E-16,1.,0.));
#10847=DIRECTION('',(-1.,0.,2.22044604925031E-16));
#10848=DIRECTION('',(2.22044604925031E-16,0.,1.));
#10849=DIRECTION('',(0.,0.,1.));
#10850=DIRECTION('',(2.22044604925031E-16,1.,0.));
#10851=DIRECTION('',(0.,0.,1.));
#10852=DIRECTION('',(2.22044604925031E-16,1.,0.));
#10853=DIRECTION('',(0.,0.,1.));
#10854=DIRECTION('',(2.22044604925031E-16,1.,0.));
#10855=DIRECTION('',(0.,0.,1.));
#10856=DIRECTION('',(2.22044604925031E-16,1.,0.));
#10857=DIRECTION('',(-1.,0.,2.22044604925031E-16));
#10858=DIRECTION('',(2.22044604925031E-16,0.,1.));
#10859=DIRECTION('',(0.,0.,1.));
#10860=DIRECTION('',(2.22044604925031E-16,1.,0.));
#10861=DIRECTION('',(0.,0.,1.));
#10862=DIRECTION('',(2.22044604925031E-16,1.,0.));
#10863=DIRECTION('',(0.,0.,1.));
#10864=DIRECTION('',(2.22044604925031E-16,1.,0.));
#10865=DIRECTION('',(-1.,0.,2.22044604925031E-16));
#10866=DIRECTION('',(2.22044604925031E-16,0.,1.));
#10867=DIRECTION('',(0.,0.,1.));
#10868=DIRECTION('',(2.22044604925031E-16,1.,0.));
#10869=DIRECTION('',(0.,0.,1.));
#10870=DIRECTION('',(2.22044604925031E-16,1.,0.));
#10871=DIRECTION('',(0.,0.,1.));
#10872=DIRECTION('',(2.22044604925031E-16,1.,0.));
#10873=DIRECTION('',(0.,0.,1.));
#10874=DIRECTION('',(2.22044604925031E-16,1.,0.));
#10875=DIRECTION('',(0.,0.,1.));
#10876=DIRECTION('',(2.22044604925031E-16,1.,0.));
#10877=DIRECTION('',(0.,0.,1.));
#10878=DIRECTION('',(1.,0.,0.));
#10879=DIRECTION('',(0.,0.,1.));
#10880=DIRECTION('',(1.,0.,0.));
#10881=DIRECTION('',(-1.,0.,2.22044604925031E-16));
#10882=DIRECTION('',(2.22044604925031E-16,0.,1.));
#10883=DIRECTION('',(0.,0.,1.));
#10884=DIRECTION('',(2.22044604925031E-16,1.,0.));
#10885=DIRECTION('',(0.,0.,1.));
#10886=DIRECTION('',(2.22044604925031E-16,1.,0.));
#10887=DIRECTION('',(0.,0.,1.));
#10888=DIRECTION('',(2.22044604925031E-16,1.,0.));
#10889=DIRECTION('',(0.,0.,1.));
#10890=DIRECTION('',(2.22044604925031E-16,1.,0.));
#10891=DIRECTION('',(0.,0.,1.));
#10892=DIRECTION('',(2.22044604925031E-16,-1.,0.));
#10893=DIRECTION('',(0.,0.,1.));
#10894=DIRECTION('',(2.22044604925031E-16,-1.,0.));
#10895=DIRECTION('',(0.,0.,1.));
#10896=DIRECTION('',(1.,0.,0.));
#10897=DIRECTION('',(0.,0.,1.));
#10898=DIRECTION('',(1.,0.,0.));
#10899=CARTESIAN_POINT('',(0.,0.,0.));
#10900=CARTESIAN_POINT('',(0.,0.,0.));
#10901=CARTESIAN_POINT('',(0.,0.,0.));
#10902=CARTESIAN_POINT('Origin',(23.,-11.,-1.1));
#10903=CARTESIAN_POINT('',(22.725,-11.,-1.));
#10904=CARTESIAN_POINT('Origin',(23.,-11.,-1.));
#10905=CARTESIAN_POINT('',(22.725,-11.,0.));
#10906=CARTESIAN_POINT('',(22.725,-11.,-1.1));
#10907=CARTESIAN_POINT('Origin',(23.,-11.,0.));
#10908=CARTESIAN_POINT('Origin',(3.,11.,-1.1));
#10909=CARTESIAN_POINT('',(2.725,11.,-1.));
#10910=CARTESIAN_POINT('Origin',(3.,11.,-1.));
#10911=CARTESIAN_POINT('',(2.725,11.,0.));
#10912=CARTESIAN_POINT('',(2.725,11.,-1.1));
#10913=CARTESIAN_POINT('Origin',(3.,11.,0.));
#10914=CARTESIAN_POINT('Origin',(3.,-11.,-1.1));
#10915=CARTESIAN_POINT('',(2.725,-11.,-1.));
#10916=CARTESIAN_POINT('Origin',(3.,-11.,-1.));
#10917=CARTESIAN_POINT('',(2.725,-11.,0.));
#10918=CARTESIAN_POINT('',(2.725,-11.,-1.1));
#10919=CARTESIAN_POINT('Origin',(3.,-11.,0.));
#10920=CARTESIAN_POINT('Origin',(23.,11.,-1.1));
#10921=CARTESIAN_POINT('',(22.725,11.,-1.));
#10922=CARTESIAN_POINT('Origin',(23.,11.,-1.));
#10923=CARTESIAN_POINT('',(22.725,11.,0.));
#10924=CARTESIAN_POINT('',(22.725,11.,-1.1));
#10925=CARTESIAN_POINT('Origin',(23.,11.,0.));
#10926=CARTESIAN_POINT('Origin',(26.,13.,-1.));
#10927=CARTESIAN_POINT('',(26.,13.,-1.));
#10928=CARTESIAN_POINT('',(0.,13.,-1.));
#10929=CARTESIAN_POINT('',(26.,13.,-1.));
#10930=CARTESIAN_POINT('',(0.,13.,0.));
#10931=CARTESIAN_POINT('',(0.,13.,-1.));
#10932=CARTESIAN_POINT('',(26.,13.,0.));
#10933=CARTESIAN_POINT('',(26.,13.,0.));
#10934=CARTESIAN_POINT('',(26.,13.,-1.));
#10935=CARTESIAN_POINT('Origin',(26.,-13.,-1.));
#10936=CARTESIAN_POINT('',(26.,-13.,-1.));
#10937=CARTESIAN_POINT('',(26.,-13.,-1.));
#10938=CARTESIAN_POINT('',(26.,-13.,0.));
#10939=CARTESIAN_POINT('',(26.,-13.,0.));
#10940=CARTESIAN_POINT('',(26.,-13.,-1.));
#10941=CARTESIAN_POINT('Origin',(0.,-13.,-1.));
#10942=CARTESIAN_POINT('',(0.,-13.,-1.));
#10943=CARTESIAN_POINT('',(0.,-13.,-1.));
#10944=CARTESIAN_POINT('',(0.,-13.,0.));
#10945=CARTESIAN_POINT('',(0.,-13.,0.));
#10946=CARTESIAN_POINT('',(0.,-13.,-1.));
#10947=CARTESIAN_POINT('Origin',(0.,13.,-1.));
#10948=CARTESIAN_POINT('',(0.,13.,-1.));
#10949=CARTESIAN_POINT('',(0.,13.,0.));
#10950=CARTESIAN_POINT('Origin',(13.,0.,0.));
#10951=CARTESIAN_POINT('Origin',(13.,0.,-1.));
#10952=CARTESIAN_POINT('',(0.,0.,0.));
#10953=CARTESIAN_POINT('Origin',(23.,-11.,39.9));
#10954=CARTESIAN_POINT('',(22.725,-11.,40.));
#10955=CARTESIAN_POINT('Origin',(23.,-11.,40.));
#10956=CARTESIAN_POINT('',(22.725,-11.,41.));
#10957=CARTESIAN_POINT('',(22.725,-11.,39.9));
#10958=CARTESIAN_POINT('Origin',(23.,-11.,41.));
#10959=CARTESIAN_POINT('Origin',(3.,11.,39.9));
#10960=CARTESIAN_POINT('',(2.725,11.,40.));
#10961=CARTESIAN_POINT('Origin',(3.,11.,40.));
#10962=CARTESIAN_POINT('',(2.725,11.,41.));
#10963=CARTESIAN_POINT('',(2.725,11.,39.9));
#10964=CARTESIAN_POINT('Origin',(3.,11.,41.));
#10965=CARTESIAN_POINT('Origin',(3.,-11.,39.9));
#10966=CARTESIAN_POINT('',(2.725,-11.,40.));
#10967=CARTESIAN_POINT('Origin',(3.,-11.,40.));
#10968=CARTESIAN_POINT('',(2.725,-11.,41.));
#10969=CARTESIAN_POINT('',(2.725,-11.,39.9));
#10970=CARTESIAN_POINT('Origin',(3.,-11.,41.));
#10971=CARTESIAN_POINT('Origin',(23.,11.,39.9));
#10972=CARTESIAN_POINT('',(22.725,11.,40.));
#10973=CARTESIAN_POINT('Origin',(23.,11.,40.));
#10974=CARTESIAN_POINT('',(22.725,11.,41.));
#10975=CARTESIAN_POINT('',(22.725,11.,39.9));
#10976=CARTESIAN_POINT('Origin',(23.,11.,41.));
#10977=CARTESIAN_POINT('Origin',(5.,-9.,39.9));
#10978=CARTESIAN_POINT('',(21.,-9.,41.));
#10979=CARTESIAN_POINT('',(5.,-9.,41.));
#10980=CARTESIAN_POINT('',(9.,-9.,41.));
#10981=CARTESIAN_POINT('',(21.,-9.,40.));
#10982=CARTESIAN_POINT('',(21.,-9.,39.9));
#10983=CARTESIAN_POINT('',(5.,-9.,40.));
#10984=CARTESIAN_POINT('',(9.,-9.,40.));
#10985=CARTESIAN_POINT('',(5.,-9.,39.9));
#10986=CARTESIAN_POINT('Origin',(5.,9.,39.9));
#10987=CARTESIAN_POINT('',(5.,9.,41.));
#10988=CARTESIAN_POINT('',(5.,4.5,41.));
#10989=CARTESIAN_POINT('',(5.,9.,40.));
#10990=CARTESIAN_POINT('',(5.,4.5,40.));
#10991=CARTESIAN_POINT('',(5.,9.,39.9));
#10992=CARTESIAN_POINT('Origin',(21.,9.,39.9));
#10993=CARTESIAN_POINT('',(21.,9.,41.));
#10994=CARTESIAN_POINT('',(17.,9.,41.));
#10995=CARTESIAN_POINT('',(21.,9.,40.));
#10996=CARTESIAN_POINT('',(17.,9.,40.));
#10997=CARTESIAN_POINT('',(21.,9.,39.9));
#10998=CARTESIAN_POINT('Origin',(21.,-9.,39.9));
#10999=CARTESIAN_POINT('',(21.,-4.5,41.));
#11000=CARTESIAN_POINT('',(21.,-4.5,40.));
#11001=CARTESIAN_POINT('Origin',(26.,13.,40.));
#11002=CARTESIAN_POINT('',(26.,13.,40.));
#11003=CARTESIAN_POINT('',(0.,13.,40.));
#11004=CARTESIAN_POINT('',(26.,13.,40.));
#11005=CARTESIAN_POINT('',(0.,13.,41.));
#11006=CARTESIAN_POINT('',(0.,13.,40.));
#11007=CARTESIAN_POINT('',(26.,13.,41.));
#11008=CARTESIAN_POINT('',(26.,13.,41.));
#11009=CARTESIAN_POINT('',(26.,13.,40.));
#11010=CARTESIAN_POINT('Origin',(26.,-13.,40.));
#11011=CARTESIAN_POINT('',(26.,-13.,40.));
#11012=CARTESIAN_POINT('',(26.,-13.,40.));
#11013=CARTESIAN_POINT('',(26.,-13.,41.));
#11014=CARTESIAN_POINT('',(26.,-13.,41.));
#11015=CARTESIAN_POINT('',(26.,-13.,40.));
#11016=CARTESIAN_POINT('Origin',(0.,-13.,40.));
#11017=CARTESIAN_POINT('',(0.,-13.,40.));
#11018=CARTESIAN_POINT('',(0.,-13.,40.));
#11019=CARTESIAN_POINT('',(0.,-13.,41.));
#11020=CARTESIAN_POINT('',(0.,-13.,41.));
#11021=CARTESIAN_POINT('',(0.,-13.,40.));
#11022=CARTESIAN_POINT('Origin',(0.,13.,40.));
#11023=CARTESIAN_POINT('',(0.,13.,40.));
#11024=CARTESIAN_POINT('',(0.,13.,41.));
#11025=CARTESIAN_POINT('Origin',(13.,0.,41.));
#11026=CARTESIAN_POINT('Origin',(13.,0.,40.));
#11027=CARTESIAN_POINT('',(0.,0.,0.));
#11028=CARTESIAN_POINT('Origin',(2.,13.,-1.8));
#11029=CARTESIAN_POINT('',(2.,13.,-1.8));
#11030=CARTESIAN_POINT('',(0.,13.,-1.8));
#11031=CARTESIAN_POINT('',(2.,13.,-1.8));
#11032=CARTESIAN_POINT('',(0.,13.,-1.));
#11033=CARTESIAN_POINT('',(0.,13.,-1.8));
#11034=CARTESIAN_POINT('',(2.,13.,-1.));
#11035=CARTESIAN_POINT('',(2.,13.,-1.));
#11036=CARTESIAN_POINT('',(2.,13.,-1.8));
#11037=CARTESIAN_POINT('Origin',(2.,-13.,-1.8));
#11038=CARTESIAN_POINT('',(2.,-13.,-1.8));
#11039=CARTESIAN_POINT('',(2.,-13.,-1.8));
#11040=CARTESIAN_POINT('',(2.,-13.,-1.));
#11041=CARTESIAN_POINT('',(2.,-13.,-1.));
#11042=CARTESIAN_POINT('',(2.,-13.,-1.8));
#11043=CARTESIAN_POINT('Origin',(0.,-13.,-1.8));
#11044=CARTESIAN_POINT('',(0.,-13.,-1.8));
#11045=CARTESIAN_POINT('',(0.,-13.,-1.8));
#11046=CARTESIAN_POINT('',(0.,-13.,-1.));
#11047=CARTESIAN_POINT('',(0.,-13.,-1.));
#11048=CARTESIAN_POINT('',(0.,-13.,-1.8));
#11049=CARTESIAN_POINT('Origin',(0.,13.,-1.8));
#11050=CARTESIAN_POINT('',(0.,13.,-1.8));
#11051=CARTESIAN_POINT('',(0.,13.,-1.));
#11052=CARTESIAN_POINT('Origin',(1.,0.,-1.));
#11053=CARTESIAN_POINT('Origin',(1.,0.,-1.8));
#11054=CARTESIAN_POINT('',(0.,0.,0.));
#11055=CARTESIAN_POINT('Origin',(26.,13.,-1.8));
#11056=CARTESIAN_POINT('',(26.,13.,-1.8));
#11057=CARTESIAN_POINT('',(24.,13.,-1.8));
#11058=CARTESIAN_POINT('',(26.,13.,-1.8));
#11059=CARTESIAN_POINT('',(24.,13.,-1.));
#11060=CARTESIAN_POINT('',(24.,13.,-1.8));
#11061=CARTESIAN_POINT('',(26.,13.,-1.));
#11062=CARTESIAN_POINT('',(26.,13.,-1.));
#11063=CARTESIAN_POINT('',(26.,13.,-1.8));
#11064=CARTESIAN_POINT('Origin',(26.,-13.,-1.8));
#11065=CARTESIAN_POINT('',(26.,-13.,-1.8));
#11066=CARTESIAN_POINT('',(26.,-13.,-1.8));
#11067=CARTESIAN_POINT('',(26.,-13.,-1.));
#11068=CARTESIAN_POINT('',(26.,-13.,-1.));
#11069=CARTESIAN_POINT('',(26.,-13.,-1.8));
#11070=CARTESIAN_POINT('Origin',(24.,-13.,-1.8));
#11071=CARTESIAN_POINT('',(24.,-13.,-1.8));
#11072=CARTESIAN_POINT('',(24.,-13.,-1.8));
#11073=CARTESIAN_POINT('',(24.,-13.,-1.));
#11074=CARTESIAN_POINT('',(24.,-13.,-1.));
#11075=CARTESIAN_POINT('',(24.,-13.,-1.8));
#11076=CARTESIAN_POINT('Origin',(24.,13.,-1.8));
#11077=CARTESIAN_POINT('',(24.,13.,-1.8));
#11078=CARTESIAN_POINT('',(24.,13.,-1.));
#11079=CARTESIAN_POINT('Origin',(25.,0.,-1.));
#11080=CARTESIAN_POINT('Origin',(25.,0.,-1.8));
#11081=CARTESIAN_POINT('',(0.,0.,0.));
#11082=CARTESIAN_POINT('Origin',(0.,-7.5,4.));
#11083=CARTESIAN_POINT('',(0.,-7.5,4.3));
#11084=CARTESIAN_POINT('',(0.,-7.5,4.));
#11085=CARTESIAN_POINT('',(0.,-7.5,4.3));
#11086=CARTESIAN_POINT('',(0.,7.5,4.3));
#11087=CARTESIAN_POINT('',(0.,-7.5,4.3));
#11088=CARTESIAN_POINT('',(0.,7.5,4.));
#11089=CARTESIAN_POINT('',(0.,7.5,4.3));
#11090=CARTESIAN_POINT('',(0.,-7.5,4.));
#11091=CARTESIAN_POINT('Origin',(25.,-7.5,10.));
#11092=CARTESIAN_POINT('',(25.,-7.5,10.));
#11093=CARTESIAN_POINT('',(0.,-7.5,4.));
#11094=CARTESIAN_POINT('',(25.,7.5,10.));
#11095=CARTESIAN_POINT('',(0.,7.5,4.));
#11096=CARTESIAN_POINT('',(25.,-7.5,10.));
#11097=CARTESIAN_POINT('Origin',(25.,-7.5,10.3));
#11098=CARTESIAN_POINT('',(25.,-7.5,10.3));
#11099=CARTESIAN_POINT('',(25.,-7.5,10.));
#11100=CARTESIAN_POINT('',(25.,7.5,10.3));
#11101=CARTESIAN_POINT('',(25.,7.5,10.));
#11102=CARTESIAN_POINT('',(25.,-7.5,10.3));
#11103=CARTESIAN_POINT('Origin',(0.,-7.5,4.3));
#11104=CARTESIAN_POINT('',(25.,-7.5,10.3));
#11105=CARTESIAN_POINT('',(25.,7.5,10.3));
#11106=CARTESIAN_POINT('Origin',(12.5,7.5,7.15));
#11107=CARTESIAN_POINT('Origin',(12.5,-7.5,7.15));
#11108=CARTESIAN_POINT('',(0.,0.,0.));
#11109=CARTESIAN_POINT('Origin',(2.3,-7.9,7.));
#11110=CARTESIAN_POINT('',(2.075,-7.8,7.));
#11111=CARTESIAN_POINT('Origin',(2.3,-7.8,7.));
#11112=CARTESIAN_POINT('',(2.075,-7.5,7.));
#11113=CARTESIAN_POINT('',(2.075,-7.9,7.));
#11114=CARTESIAN_POINT('Origin',(2.3,-7.5,7.));
#11115=CARTESIAN_POINT('Origin',(22.3,-7.9,12.));
#11116=CARTESIAN_POINT('',(22.075,-7.8,12.));
#11117=CARTESIAN_POINT('Origin',(22.3,-7.8,12.));
#11118=CARTESIAN_POINT('',(22.075,-7.5,12.));
#11119=CARTESIAN_POINT('',(22.075,-7.9,12.));
#11120=CARTESIAN_POINT('Origin',(22.3,-7.5,12.));
#11121=CARTESIAN_POINT('Origin',(0.,-7.8,4.));
#11122=CARTESIAN_POINT('',(0.,-7.8,16.));
#11123=CARTESIAN_POINT('',(0.,-7.8,4.));
#11124=CARTESIAN_POINT('',(0.,-7.8,16.));
#11125=CARTESIAN_POINT('',(0.,-7.5,16.));
#11126=CARTESIAN_POINT('',(0.,-7.8,16.));
#11127=CARTESIAN_POINT('',(0.,-7.5,4.));
#11128=CARTESIAN_POINT('',(0.,-7.5,16.));
#11129=CARTESIAN_POINT('',(0.,-7.8,4.));
#11130=CARTESIAN_POINT('Origin',(25.,-7.8,10.));
#11131=CARTESIAN_POINT('',(25.,-7.8,10.));
#11132=CARTESIAN_POINT('',(0.,-7.8,4.));
#11133=CARTESIAN_POINT('',(25.,-7.5,10.));
#11134=CARTESIAN_POINT('',(0.,-7.5,4.));
#11135=CARTESIAN_POINT('',(25.,-7.8,10.));
#11136=CARTESIAN_POINT('Origin',(25.,-7.8,18.));
#11137=CARTESIAN_POINT('',(25.,-7.8,18.));
#11138=CARTESIAN_POINT('',(25.,-7.8,10.));
#11139=CARTESIAN_POINT('',(25.,-7.5,18.));
#11140=CARTESIAN_POINT('',(25.,-7.5,10.));
#11141=CARTESIAN_POINT('',(25.,-7.8,18.));
#11142=CARTESIAN_POINT('Origin',(0.,-7.8,16.));
#11143=CARTESIAN_POINT('',(25.,-7.8,18.));
#11144=CARTESIAN_POINT('',(25.,-7.5,18.));
#11145=CARTESIAN_POINT('Origin',(12.5,-7.5,11.));
#11146=CARTESIAN_POINT('Origin',(12.5,-7.8,11.));
#11147=CARTESIAN_POINT('',(0.,0.,0.));
#11148=CARTESIAN_POINT('Origin',(2.3,7.4,7.));
#11149=CARTESIAN_POINT('',(2.075,7.5,7.));
#11150=CARTESIAN_POINT('Origin',(2.3,7.5,7.));
#11151=CARTESIAN_POINT('',(2.075,7.8,7.));
#11152=CARTESIAN_POINT('',(2.075,7.4,7.));
#11153=CARTESIAN_POINT('Origin',(2.3,7.8,7.));
#11154=CARTESIAN_POINT('Origin',(22.3,7.4,12.));
#11155=CARTESIAN_POINT('',(22.075,7.5,12.));
#11156=CARTESIAN_POINT('Origin',(22.3,7.5,12.));
#11157=CARTESIAN_POINT('',(22.075,7.8,12.));
#11158=CARTESIAN_POINT('',(22.075,7.4,12.));
#11159=CARTESIAN_POINT('Origin',(22.3,7.8,12.));
#11160=CARTESIAN_POINT('Origin',(0.,7.5,4.));
#11161=CARTESIAN_POINT('',(0.,7.5,16.));
#11162=CARTESIAN_POINT('',(0.,7.5,4.));
#11163=CARTESIAN_POINT('',(0.,7.5,16.));
#11164=CARTESIAN_POINT('',(0.,7.8,16.));
#11165=CARTESIAN_POINT('',(0.,7.5,16.));
#11166=CARTESIAN_POINT('',(0.,7.8,4.));
#11167=CARTESIAN_POINT('',(0.,7.8,16.));
#11168=CARTESIAN_POINT('',(0.,7.5,4.));
#11169=CARTESIAN_POINT('Origin',(25.,7.5,10.));
#11170=CARTESIAN_POINT('',(25.,7.5,10.));
#11171=CARTESIAN_POINT('',(0.,7.5,4.));
#11172=CARTESIAN_POINT('',(25.,7.8,10.));
#11173=CARTESIAN_POINT('',(0.,7.8,4.));
#11174=CARTESIAN_POINT('',(25.,7.5,10.));
#11175=CARTESIAN_POINT('Origin',(25.,7.5,18.));
#11176=CARTESIAN_POINT('',(25.,7.5,18.));
#11177=CARTESIAN_POINT('',(25.,7.5,10.));
#11178=CARTESIAN_POINT('',(25.,7.8,18.));
#11179=CARTESIAN_POINT('',(25.,7.8,10.));
#11180=CARTESIAN_POINT('',(25.,7.5,18.));
#11181=CARTESIAN_POINT('Origin',(0.,7.5,16.));
#11182=CARTESIAN_POINT('',(25.,7.5,18.));
#11183=CARTESIAN_POINT('',(25.,7.8,18.));
#11184=CARTESIAN_POINT('Origin',(12.5,7.8,11.));
#11185=CARTESIAN_POINT('Origin',(12.5,7.5,11.));
#11186=CARTESIAN_POINT('',(0.,0.,0.));
#11187=CARTESIAN_POINT('Origin',(2.3,-9.4,7.));
#11188=CARTESIAN_POINT('',(2.135,-9.4,7.));
#11189=CARTESIAN_POINT('Origin',(2.3,-9.4,7.));
#11190=CARTESIAN_POINT('',(2.135,-7.8,7.));
#11191=CARTESIAN_POINT('',(2.135,-9.4,7.));
#11192=CARTESIAN_POINT('Origin',(2.3,-7.8,7.));
#11193=CARTESIAN_POINT('Origin',(2.3,-9.4,7.));
#11194=CARTESIAN_POINT('Origin',(3.,-8.5,7.));
#11195=CARTESIAN_POINT('',(2.5,-8.5,7.));
#11196=CARTESIAN_POINT('Origin',(3.,-8.5,7.));
#11197=CARTESIAN_POINT('',(2.5,-7.8,7.));
#11198=CARTESIAN_POINT('',(2.5,-8.5,7.));
#11199=CARTESIAN_POINT('Origin',(3.,-7.8,7.));
#11200=CARTESIAN_POINT('Origin',(3.,-8.5,7.));
#11201=CARTESIAN_POINT('',(2.725,-8.5,7.));
#11202=CARTESIAN_POINT('Origin',(3.,-8.5,7.));
#11203=CARTESIAN_POINT('Origin',(3.,-10.1,7.));
#11204=CARTESIAN_POINT('',(2.725,-10.,7.));
#11205=CARTESIAN_POINT('Origin',(3.,-10.,7.));
#11206=CARTESIAN_POINT('',(2.725,-10.1,7.));
#11207=CARTESIAN_POINT('Origin',(4.,-7.8,6.));
#11208=CARTESIAN_POINT('',(4.,-7.8,6.));
#11209=CARTESIAN_POINT('',(2.,-7.8,6.));
#11210=CARTESIAN_POINT('',(4.,-7.8,6.));
#11211=CARTESIAN_POINT('',(2.,-7.8,8.));
#11212=CARTESIAN_POINT('',(2.,-7.8,6.));
#11213=CARTESIAN_POINT('',(4.,-7.8,8.));
#11214=CARTESIAN_POINT('',(4.,-7.8,8.));
#11215=CARTESIAN_POINT('',(4.,-7.8,6.));
#11216=CARTESIAN_POINT('Origin',(4.,-10.,6.));
#11217=CARTESIAN_POINT('',(4.,-10.,6.));
#11218=CARTESIAN_POINT('',(4.,-10.,6.));
#11219=CARTESIAN_POINT('',(4.,-10.,8.));
#11220=CARTESIAN_POINT('',(4.,-10.,8.));
#11221=CARTESIAN_POINT('',(4.,-10.,6.));
#11222=CARTESIAN_POINT('Origin',(2.,-10.,6.));
#11223=CARTESIAN_POINT('',(2.,-10.,6.));
#11224=CARTESIAN_POINT('',(2.,-10.,6.));
#11225=CARTESIAN_POINT('',(2.,-10.,8.));
#11226=CARTESIAN_POINT('',(2.,-10.,8.));
#11227=CARTESIAN_POINT('',(2.,-10.,6.));
#11228=CARTESIAN_POINT('Origin',(2.,-7.8,6.));
#11229=CARTESIAN_POINT('',(2.,-7.8,6.));
#11230=CARTESIAN_POINT('',(2.,-7.8,8.));
#11231=CARTESIAN_POINT('Origin',(3.,-8.9,8.));
#11232=CARTESIAN_POINT('Origin',(3.,-8.9,6.));
#11233=CARTESIAN_POINT('',(0.,0.,0.));
#11234=CARTESIAN_POINT('Origin',(2.3,7.7,7.));
#11235=CARTESIAN_POINT('',(2.135,7.8,7.));
#11236=CARTESIAN_POINT('Origin',(2.3,7.8,7.));
#11237=CARTESIAN_POINT('',(2.135,9.4,7.));
#11238=CARTESIAN_POINT('',(2.135,7.7,7.));
#11239=CARTESIAN_POINT('Origin',(2.3,9.4,7.));
#11240=CARTESIAN_POINT('Origin',(2.3,9.4,7.));
#11241=CARTESIAN_POINT('Origin',(3.,7.7,7.));
#11242=CARTESIAN_POINT('',(2.5,7.8,7.));
#11243=CARTESIAN_POINT('Origin',(3.,7.8,7.));
#11244=CARTESIAN_POINT('',(2.5,8.5,7.));
#11245=CARTESIAN_POINT('',(2.5,7.7,7.));
#11246=CARTESIAN_POINT('Origin',(3.,8.5,7.));
#11247=CARTESIAN_POINT('Origin',(3.,8.5,7.));
#11248=CARTESIAN_POINT('',(2.725,8.5,7.));
#11249=CARTESIAN_POINT('Origin',(3.,8.5,7.));
#11250=CARTESIAN_POINT('Origin',(3.,7.7,7.));
#11251=CARTESIAN_POINT('',(2.725,10.,7.));
#11252=CARTESIAN_POINT('',(2.725,7.7,7.));
#11253=CARTESIAN_POINT('Origin',(3.,10.,7.));
#11254=CARTESIAN_POINT('Origin',(4.,10.,6.));
#11255=CARTESIAN_POINT('',(4.,10.,6.));
#11256=CARTESIAN_POINT('',(2.,10.,6.));
#11257=CARTESIAN_POINT('',(4.,10.,6.));
#11258=CARTESIAN_POINT('',(2.,10.,8.));
#11259=CARTESIAN_POINT('',(2.,10.,6.));
#11260=CARTESIAN_POINT('',(4.,10.,8.));
#11261=CARTESIAN_POINT('',(4.,10.,8.));
#11262=CARTESIAN_POINT('',(4.,10.,6.));
#11263=CARTESIAN_POINT('Origin',(4.,7.8,6.));
#11264=CARTESIAN_POINT('',(4.,7.8,6.));
#11265=CARTESIAN_POINT('',(4.,7.8,6.));
#11266=CARTESIAN_POINT('',(4.,7.8,8.));
#11267=CARTESIAN_POINT('',(4.,7.8,8.));
#11268=CARTESIAN_POINT('',(4.,7.8,6.));
#11269=CARTESIAN_POINT('Origin',(2.,7.8,6.));
#11270=CARTESIAN_POINT('',(2.,7.8,6.));
#11271=CARTESIAN_POINT('',(2.,7.8,6.));
#11272=CARTESIAN_POINT('',(2.,7.8,8.));
#11273=CARTESIAN_POINT('',(2.,7.8,8.));
#11274=CARTESIAN_POINT('',(2.,7.8,6.));
#11275=CARTESIAN_POINT('Origin',(2.,10.,6.));
#11276=CARTESIAN_POINT('',(2.,10.,6.));
#11277=CARTESIAN_POINT('',(2.,10.,8.));
#11278=CARTESIAN_POINT('Origin',(3.,8.9,8.));
#11279=CARTESIAN_POINT('Origin',(3.,8.9,6.));
#11280=CARTESIAN_POINT('',(0.,0.,0.));
#11281=CARTESIAN_POINT('Origin',(22.3,-9.4,12.));
#11282=CARTESIAN_POINT('',(22.135,-9.4,12.));
#11283=CARTESIAN_POINT('Origin',(22.3,-9.4,12.));
#11284=CARTESIAN_POINT('',(22.135,-7.8,12.));
#11285=CARTESIAN_POINT('',(22.135,-9.4,12.));
#11286=CARTESIAN_POINT('Origin',(22.3,-7.8,12.));
#11287=CARTESIAN_POINT('Origin',(22.3,-9.4,12.));
#11288=CARTESIAN_POINT('Origin',(23.,-8.5,12.));
#11289=CARTESIAN_POINT('',(22.5,-8.5,12.));
#11290=CARTESIAN_POINT('Origin',(23.,-8.5,12.));
#11291=CARTESIAN_POINT('',(22.5,-7.8,12.));
#11292=CARTESIAN_POINT('',(22.5,-8.5,12.));
#11293=CARTESIAN_POINT('Origin',(23.,-7.8,12.));
#11294=CARTESIAN_POINT('Origin',(23.,-8.5,12.));
#11295=CARTESIAN_POINT('',(22.725,-8.5,12.));
#11296=CARTESIAN_POINT('Origin',(23.,-8.5,12.));
#11297=CARTESIAN_POINT('Origin',(23.,-10.1,12.));
#11298=CARTESIAN_POINT('',(22.725,-10.,12.));
#11299=CARTESIAN_POINT('Origin',(23.,-10.,12.));
#11300=CARTESIAN_POINT('',(22.725,-10.1,12.));
#11301=CARTESIAN_POINT('Origin',(24.,-7.8,11.));
#11302=CARTESIAN_POINT('',(24.,-7.8,11.));
#11303=CARTESIAN_POINT('',(22.,-7.8,11.));
#11304=CARTESIAN_POINT('',(24.,-7.8,11.));
#11305=CARTESIAN_POINT('',(22.,-7.8,13.));
#11306=CARTESIAN_POINT('',(22.,-7.8,11.));
#11307=CARTESIAN_POINT('',(24.,-7.8,13.));
#11308=CARTESIAN_POINT('',(24.,-7.8,13.));
#11309=CARTESIAN_POINT('',(24.,-7.8,11.));
#11310=CARTESIAN_POINT('Origin',(24.,-10.,11.));
#11311=CARTESIAN_POINT('',(24.,-10.,11.));
#11312=CARTESIAN_POINT('',(24.,-10.,11.));
#11313=CARTESIAN_POINT('',(24.,-10.,13.));
#11314=CARTESIAN_POINT('',(24.,-10.,13.));
#11315=CARTESIAN_POINT('',(24.,-10.,11.));
#11316=CARTESIAN_POINT('Origin',(22.,-10.,11.));
#11317=CARTESIAN_POINT('',(22.,-10.,11.));
#11318=CARTESIAN_POINT('',(22.,-10.,11.));
#11319=CARTESIAN_POINT('',(22.,-10.,13.));
#11320=CARTESIAN_POINT('',(22.,-10.,13.));
#11321=CARTESIAN_POINT('',(22.,-10.,11.));
#11322=CARTESIAN_POINT('Origin',(22.,-7.8,11.));
#11323=CARTESIAN_POINT('',(22.,-7.8,11.));
#11324=CARTESIAN_POINT('',(22.,-7.8,13.));
#11325=CARTESIAN_POINT('Origin',(23.,-8.9,13.));
#11326=CARTESIAN_POINT('Origin',(23.,-8.9,11.));
#11327=CARTESIAN_POINT('',(0.,0.,0.));
#11328=CARTESIAN_POINT('Origin',(22.3,7.7,12.));
#11329=CARTESIAN_POINT('',(22.135,7.8,12.));
#11330=CARTESIAN_POINT('Origin',(22.3,7.8,12.));
#11331=CARTESIAN_POINT('',(22.135,9.4,12.));
#11332=CARTESIAN_POINT('',(22.135,7.7,12.));
#11333=CARTESIAN_POINT('Origin',(22.3,9.4,12.));
#11334=CARTESIAN_POINT('Origin',(22.3,9.4,12.));
#11335=CARTESIAN_POINT('Origin',(23.,7.7,12.));
#11336=CARTESIAN_POINT('',(22.5,7.8,12.));
#11337=CARTESIAN_POINT('Origin',(23.,7.8,12.));
#11338=CARTESIAN_POINT('',(22.5,8.5,12.));
#11339=CARTESIAN_POINT('',(22.5,7.7,12.));
#11340=CARTESIAN_POINT('Origin',(23.,8.5,12.));
#11341=CARTESIAN_POINT('Origin',(23.,8.5,12.));
#11342=CARTESIAN_POINT('',(22.725,8.5,12.));
#11343=CARTESIAN_POINT('Origin',(23.,8.5,12.));
#11344=CARTESIAN_POINT('Origin',(23.,7.7,12.));
#11345=CARTESIAN_POINT('',(22.725,10.,12.));
#11346=CARTESIAN_POINT('',(22.725,7.7,12.));
#11347=CARTESIAN_POINT('Origin',(23.,10.,12.));
#11348=CARTESIAN_POINT('Origin',(24.,10.,11.));
#11349=CARTESIAN_POINT('',(24.,10.,11.));
#11350=CARTESIAN_POINT('',(22.,10.,11.));
#11351=CARTESIAN_POINT('',(24.,10.,11.));
#11352=CARTESIAN_POINT('',(22.,10.,13.));
#11353=CARTESIAN_POINT('',(22.,10.,11.));
#11354=CARTESIAN_POINT('',(24.,10.,13.));
#11355=CARTESIAN_POINT('',(24.,10.,13.));
#11356=CARTESIAN_POINT('',(24.,10.,11.));
#11357=CARTESIAN_POINT('Origin',(24.,7.8,11.));
#11358=CARTESIAN_POINT('',(24.,7.8,11.));
#11359=CARTESIAN_POINT('',(24.,7.8,11.));
#11360=CARTESIAN_POINT('',(24.,7.8,13.));
#11361=CARTESIAN_POINT('',(24.,7.8,13.));
#11362=CARTESIAN_POINT('',(24.,7.8,11.));
#11363=CARTESIAN_POINT('Origin',(22.,7.8,11.));
#11364=CARTESIAN_POINT('',(22.,7.8,11.));
#11365=CARTESIAN_POINT('',(22.,7.8,11.));
#11366=CARTESIAN_POINT('',(22.,7.8,13.));
#11367=CARTESIAN_POINT('',(22.,7.8,13.));
#11368=CARTESIAN_POINT('',(22.,7.8,11.));
#11369=CARTESIAN_POINT('Origin',(22.,10.,11.));
#11370=CARTESIAN_POINT('',(22.,10.,11.));
#11371=CARTESIAN_POINT('',(22.,10.,13.));
#11372=CARTESIAN_POINT('Origin',(23.,8.9,13.));
#11373=CARTESIAN_POINT('Origin',(23.,8.9,11.));
#11374=CARTESIAN_POINT('',(0.,0.,0.));
#11375=CARTESIAN_POINT('Origin',(-1.1,-7.5,4.3));
#11376=CARTESIAN_POINT('',(0.,7.5,4.3));
#11377=CARTESIAN_POINT('',(0.,-7.5,4.3));
#11378=CARTESIAN_POINT('',(0.,-3.75,4.3));
#11379=CARTESIAN_POINT('',(-1.,7.5,4.3));
#11380=CARTESIAN_POINT('',(-1.1,7.5,4.3));
#11381=CARTESIAN_POINT('',(-1.,-7.5,4.3));
#11382=CARTESIAN_POINT('',(-1.,-3.75,4.3));
#11383=CARTESIAN_POINT('',(-1.1,-7.5,4.3));
#11384=CARTESIAN_POINT('Origin',(-1.1,-7.5,16.));
#11385=CARTESIAN_POINT('',(0.,-7.5,16.));
#11386=CARTESIAN_POINT('',(0.,-7.5,13.));
#11387=CARTESIAN_POINT('',(-1.,-7.5,16.));
#11388=CARTESIAN_POINT('',(-1.,-7.5,13.));
#11389=CARTESIAN_POINT('',(-1.1,-7.5,16.));
#11390=CARTESIAN_POINT('Origin',(-1.1,7.5,16.));
#11391=CARTESIAN_POINT('',(0.,7.5,16.));
#11392=CARTESIAN_POINT('',(0.,3.75,16.));
#11393=CARTESIAN_POINT('',(-1.,7.5,16.));
#11394=CARTESIAN_POINT('',(-1.,3.75,16.));
#11395=CARTESIAN_POINT('',(-1.1,7.5,16.));
#11396=CARTESIAN_POINT('Origin',(-1.1,7.5,4.3));
#11397=CARTESIAN_POINT('',(0.,7.5,7.15));
#11398=CARTESIAN_POINT('',(-1.,7.5,7.15));
#11399=CARTESIAN_POINT('Origin',(-1.,8.5,17.));
#11400=CARTESIAN_POINT('',(-1.,8.5,17.));
#11401=CARTESIAN_POINT('',(-1.,-8.5,17.));
#11402=CARTESIAN_POINT('',(-1.,8.5,17.));
#11403=CARTESIAN_POINT('',(0.,-8.5,17.));
#11404=CARTESIAN_POINT('',(-1.,-8.5,17.));
#11405=CARTESIAN_POINT('',(0.,8.5,17.));
#11406=CARTESIAN_POINT('',(0.,8.5,17.));
#11407=CARTESIAN_POINT('',(-1.,8.5,17.));
#11408=CARTESIAN_POINT('Origin',(-1.,8.5,3.));
#11409=CARTESIAN_POINT('',(-1.,8.5,3.));
#11410=CARTESIAN_POINT('',(-1.,8.5,3.));
#11411=CARTESIAN_POINT('',(0.,8.5,3.));
#11412=CARTESIAN_POINT('',(0.,8.5,3.));
#11413=CARTESIAN_POINT('',(-1.,8.5,3.));
#11414=CARTESIAN_POINT('Origin',(-1.,-8.5,3.));
#11415=CARTESIAN_POINT('',(-1.,-8.5,3.));
#11416=CARTESIAN_POINT('',(-1.,-8.5,3.));
#11417=CARTESIAN_POINT('',(0.,-8.5,3.));
#11418=CARTESIAN_POINT('',(0.,-8.5,3.));
#11419=CARTESIAN_POINT('',(-1.,-8.5,3.));
#11420=CARTESIAN_POINT('Origin',(-1.,-8.5,17.));
#11421=CARTESIAN_POINT('',(-1.,-8.5,17.));
#11422=CARTESIAN_POINT('',(0.,-8.5,17.));
#11423=CARTESIAN_POINT('Origin',(0.,0.,10.));
#11424=CARTESIAN_POINT('Origin',(-1.,0.,10.));
#11425=CARTESIAN_POINT('',(0.,0.,0.));
#11426=CARTESIAN_POINT('Origin',(-1.3,-7.5,4.3));
#11427=CARTESIAN_POINT('',(-1.,7.5,4.3));
#11428=CARTESIAN_POINT('',(-1.,-7.5,4.3));
#11429=CARTESIAN_POINT('',(-1.,-3.625,4.3));
#11430=CARTESIAN_POINT('',(-1.2,7.5,4.3));
#11431=CARTESIAN_POINT('',(-1.3,7.5,4.3));
#11432=CARTESIAN_POINT('',(-1.2,-7.5,4.3));
#11433=CARTESIAN_POINT('',(-1.2,-3.625,4.3));
#11434=CARTESIAN_POINT('',(-1.3,-7.5,4.3));
#11435=CARTESIAN_POINT('Origin',(-1.3,-7.5,16.));
#11436=CARTESIAN_POINT('',(-1.,-7.5,16.));
#11437=CARTESIAN_POINT('',(-1.,-7.5,13.));
#11438=CARTESIAN_POINT('',(-1.2,-7.5,16.));
#11439=CARTESIAN_POINT('',(-1.2,-7.5,13.));
#11440=CARTESIAN_POINT('',(-1.3,-7.5,16.));
#11441=CARTESIAN_POINT('Origin',(-1.3,7.5,16.));
#11442=CARTESIAN_POINT('',(-1.,7.5,16.));
#11443=CARTESIAN_POINT('',(-1.,3.875,16.));
#11444=CARTESIAN_POINT('',(-1.2,7.5,16.));
#11445=CARTESIAN_POINT('',(-1.2,3.875,16.));
#11446=CARTESIAN_POINT('',(-1.3,7.5,16.));
#11447=CARTESIAN_POINT('Origin',(-1.3,7.5,4.3));
#11448=CARTESIAN_POINT('',(-1.,7.5,7.15));
#11449=CARTESIAN_POINT('',(-1.2,7.5,7.15));
#11450=CARTESIAN_POINT('Origin',(-1.2,8.5,17.));
#11451=CARTESIAN_POINT('',(-1.2,8.5,17.));
#11452=CARTESIAN_POINT('',(-1.2,-8.,17.));
#11453=CARTESIAN_POINT('',(-1.2,8.5,17.));
#11454=CARTESIAN_POINT('',(-1.,-8.,17.));
#11455=CARTESIAN_POINT('',(-1.2,-8.,17.));
#11456=CARTESIAN_POINT('',(-1.,8.5,17.));
#11457=CARTESIAN_POINT('',(-1.,8.5,17.));
#11458=CARTESIAN_POINT('',(-1.2,8.5,17.));
#11459=CARTESIAN_POINT('Origin',(-1.2,8.5,3.));
#11460=CARTESIAN_POINT('',(-1.2,8.5,3.));
#11461=CARTESIAN_POINT('',(-1.2,8.5,3.));
#11462=CARTESIAN_POINT('',(-1.,8.5,3.));
#11463=CARTESIAN_POINT('',(-1.,8.5,3.));
#11464=CARTESIAN_POINT('',(-1.2,8.5,3.));
#11465=CARTESIAN_POINT('Origin',(-1.2,-8.,3.));
#11466=CARTESIAN_POINT('',(-1.2,-8.,3.));
#11467=CARTESIAN_POINT('',(-1.2,-8.,3.));
#11468=CARTESIAN_POINT('',(-1.,-8.,3.));
#11469=CARTESIAN_POINT('',(-1.,-8.,3.));
#11470=CARTESIAN_POINT('',(-1.2,-8.,3.));
#11471=CARTESIAN_POINT('Origin',(-1.2,-8.,17.));
#11472=CARTESIAN_POINT('',(-1.2,-8.,17.));
#11473=CARTESIAN_POINT('',(-1.,-8.,17.));
#11474=CARTESIAN_POINT('Origin',(-1.,0.25,10.));
#11475=CARTESIAN_POINT('Origin',(-1.2,0.25,10.));
#11476=CARTESIAN_POINT('',(0.,0.,0.));
#11477=CARTESIAN_POINT('Origin',(1.1,11.,30.25));
#11478=CARTESIAN_POINT('',(1.2,11.,30.46));
#11479=CARTESIAN_POINT('Origin',(1.2,11.,30.25));
#11480=CARTESIAN_POINT('',(2.,11.,30.46));
#11481=CARTESIAN_POINT('',(1.1,11.,30.46));
#11482=CARTESIAN_POINT('Origin',(2.,11.,30.25));
#11483=CARTESIAN_POINT('Origin',(1.1,11.,6.95));
#11484=CARTESIAN_POINT('',(1.2,11.,7.16));
#11485=CARTESIAN_POINT('Origin',(1.2,11.,6.95));
#11486=CARTESIAN_POINT('',(2.,11.,7.16));
#11487=CARTESIAN_POINT('',(1.1,11.,7.16));
#11488=CARTESIAN_POINT('Origin',(2.,11.,6.95));
#11489=CARTESIAN_POINT('Origin',(1.1,11.,21.5));
#11490=CARTESIAN_POINT('',(1.2,11.,21.665));
#11491=CARTESIAN_POINT('Origin',(1.2,11.,21.5));
#11492=CARTESIAN_POINT('',(2.,11.,21.665));
#11493=CARTESIAN_POINT('',(1.1,11.,21.665));
#11494=CARTESIAN_POINT('Origin',(2.,11.,21.5));
#11495=CARTESIAN_POINT('Origin',(1.1,11.,15.5));
#11496=CARTESIAN_POINT('',(1.2,11.,15.665));
#11497=CARTESIAN_POINT('Origin',(1.2,11.,15.5));
#11498=CARTESIAN_POINT('',(2.,11.,15.665));
#11499=CARTESIAN_POINT('',(1.1,11.,15.665));
#11500=CARTESIAN_POINT('Origin',(2.,11.,15.5));
#11501=CARTESIAN_POINT('Origin',(1.1,11.,9.5));
#11502=CARTESIAN_POINT('',(1.2,11.,9.665));
#11503=CARTESIAN_POINT('Origin',(1.2,11.,9.5));
#11504=CARTESIAN_POINT('',(2.,11.,9.665));
#11505=CARTESIAN_POINT('',(1.1,11.,9.665));
#11506=CARTESIAN_POINT('Origin',(2.,11.,9.5));
#11507=CARTESIAN_POINT('Origin',(1.1,11.,27.5));
#11508=CARTESIAN_POINT('',(1.2,11.,27.665));
#11509=CARTESIAN_POINT('Origin',(1.2,11.,27.5));
#11510=CARTESIAN_POINT('',(2.,11.,27.665));
#11511=CARTESIAN_POINT('',(1.1,11.,27.665));
#11512=CARTESIAN_POINT('Origin',(2.,11.,27.5));
#11513=CARTESIAN_POINT('Origin',(1.1,11.,6.));
#11514=CARTESIAN_POINT('',(1.2,11.,6.275));
#11515=CARTESIAN_POINT('Origin',(1.2,11.,6.));
#11516=CARTESIAN_POINT('',(2.,11.,6.275));
#11517=CARTESIAN_POINT('',(1.1,11.,6.275));
#11518=CARTESIAN_POINT('Origin',(2.,11.,6.));
#11519=CARTESIAN_POINT('Origin',(1.1,11.,31.5));
#11520=CARTESIAN_POINT('',(1.2,11.,31.775));
#11521=CARTESIAN_POINT('Origin',(1.2,11.,31.5));
#11522=CARTESIAN_POINT('',(2.,11.,31.775));
#11523=CARTESIAN_POINT('',(1.1,11.,31.775));
#11524=CARTESIAN_POINT('Origin',(2.,11.,31.5));
#11525=CARTESIAN_POINT('Origin',(2.,12.,5.));
#11526=CARTESIAN_POINT('',(2.,12.,5.));
#11527=CARTESIAN_POINT('',(1.2,12.,5.));
#11528=CARTESIAN_POINT('',(2.,12.,5.));
#11529=CARTESIAN_POINT('',(1.2,12.,32.));
#11530=CARTESIAN_POINT('',(1.2,12.,5.));
#11531=CARTESIAN_POINT('',(2.,12.,32.));
#11532=CARTESIAN_POINT('',(2.,12.,32.));
#11533=CARTESIAN_POINT('',(2.,12.,5.));
#11534=CARTESIAN_POINT('Origin',(2.,10.,5.));
#11535=CARTESIAN_POINT('',(2.,10.,5.));
#11536=CARTESIAN_POINT('',(2.,10.,5.));
#11537=CARTESIAN_POINT('',(2.,10.,32.));
#11538=CARTESIAN_POINT('',(2.,10.,32.));
#11539=CARTESIAN_POINT('',(2.,10.,5.));
#11540=CARTESIAN_POINT('Origin',(1.2,10.,5.));
#11541=CARTESIAN_POINT('',(1.2,10.,5.));
#11542=CARTESIAN_POINT('',(1.2,10.,5.));
#11543=CARTESIAN_POINT('',(1.2,10.,32.));
#11544=CARTESIAN_POINT('',(1.2,10.,32.));
#11545=CARTESIAN_POINT('',(1.2,10.,5.));
#11546=CARTESIAN_POINT('Origin',(1.2,12.,5.));
#11547=CARTESIAN_POINT('',(1.2,12.,5.));
#11548=CARTESIAN_POINT('',(1.2,12.,32.));
#11549=CARTESIAN_POINT('Origin',(1.6,11.,32.));
#11550=CARTESIAN_POINT('Origin',(1.6,11.,5.));
#11551=CARTESIAN_POINT('',(0.,0.,0.));
#11552=CARTESIAN_POINT('Origin',(-2.1,-8.4,30.3));
#11553=CARTESIAN_POINT('',(-2.,-8.4,30.525));
#11554=CARTESIAN_POINT('Origin',(-2.,-8.4,30.3));
#11555=CARTESIAN_POINT('',(-1.,-8.4,30.525));
#11556=CARTESIAN_POINT('',(-2.1,-8.4,30.525));
#11557=CARTESIAN_POINT('Origin',(-1.,-8.4,30.3));
#11558=CARTESIAN_POINT('Origin',(-2.1,-8.4,18.3));
#11559=CARTESIAN_POINT('',(-2.,-8.4,18.525));
#11560=CARTESIAN_POINT('Origin',(-2.,-8.4,18.3));
#11561=CARTESIAN_POINT('',(-1.,-8.4,18.525));
#11562=CARTESIAN_POINT('',(-2.1,-8.4,18.525));
#11563=CARTESIAN_POINT('Origin',(-1.,-8.4,18.3));
#11564=CARTESIAN_POINT('Origin',(-1.6,-7.6,3.));
#11565=CARTESIAN_POINT('',(-1.6,-7.6,3.));
#11566=CARTESIAN_POINT('',(-2.,-7.6,3.));
#11567=CARTESIAN_POINT('',(-1.6,-7.6,3.));
#11568=CARTESIAN_POINT('',(-2.,-7.6,33.));
#11569=CARTESIAN_POINT('',(-2.,-7.6,3.));
#11570=CARTESIAN_POINT('',(-1.6,-7.6,33.));
#11571=CARTESIAN_POINT('',(-1.6,-7.6,33.));
#11572=CARTESIAN_POINT('',(-1.6,-7.6,3.));
#11573=CARTESIAN_POINT('Origin',(-1.6,-8.,3.));
#11574=CARTESIAN_POINT('',(-1.6,-8.,3.));
#11575=CARTESIAN_POINT('',(-1.6,-8.,3.));
#11576=CARTESIAN_POINT('',(-1.6,-8.,33.));
#11577=CARTESIAN_POINT('',(-1.6,-8.,33.));
#11578=CARTESIAN_POINT('',(-1.6,-8.,3.));
#11579=CARTESIAN_POINT('Origin',(-1.,-8.,3.));
#11580=CARTESIAN_POINT('',(-1.,-8.,3.));
#11581=CARTESIAN_POINT('',(-1.,-8.,3.));
#11582=CARTESIAN_POINT('',(-1.,-8.,33.));
#11583=CARTESIAN_POINT('',(-1.,-8.,33.));
#11584=CARTESIAN_POINT('',(-1.,-8.,3.));
#11585=CARTESIAN_POINT('Origin',(-1.,-8.8,3.));
#11586=CARTESIAN_POINT('',(-1.,-8.8,3.));
#11587=CARTESIAN_POINT('',(-1.,-8.8,3.));
#11588=CARTESIAN_POINT('',(-1.,-8.8,33.));
#11589=CARTESIAN_POINT('',(-1.,-8.8,33.));
#11590=CARTESIAN_POINT('',(-1.,-8.8,3.));
#11591=CARTESIAN_POINT('Origin',(-2.,-8.8,3.));
#11592=CARTESIAN_POINT('',(-2.,-8.8,3.));
#11593=CARTESIAN_POINT('',(-2.,-8.8,3.));
#11594=CARTESIAN_POINT('',(-2.,-8.8,33.));
#11595=CARTESIAN_POINT('',(-2.,-8.8,33.));
#11596=CARTESIAN_POINT('',(-2.,-8.8,3.));
#11597=CARTESIAN_POINT('Origin',(-2.,-7.6,3.));
#11598=CARTESIAN_POINT('',(-2.,-7.6,3.));
#11599=CARTESIAN_POINT('',(-2.,-7.6,33.));
#11600=CARTESIAN_POINT('Origin',(-1.5,-8.2,33.));
#11601=CARTESIAN_POINT('Origin',(-1.5,-8.2,3.));
#11602=CARTESIAN_POINT('',(0.,0.,0.));
#11603=CARTESIAN_POINT('Origin',(-1.1,-8.4,18.3));
#11604=CARTESIAN_POINT('',(-1.,-8.4,18.465));
#11605=CARTESIAN_POINT('Origin',(-1.,-8.4,18.3));
#11606=CARTESIAN_POINT('',(0.4,-8.4,18.465));
#11607=CARTESIAN_POINT('',(-1.1,-8.4,18.465));
#11608=CARTESIAN_POINT('Origin',(0.4,-8.4,18.3));
#11609=CARTESIAN_POINT('Origin',(0.4,-8.4,18.3));
#11610=CARTESIAN_POINT('Origin',(1.1,-11.,19.));
#11611=CARTESIAN_POINT('',(1.2,-11.,19.275));
#11612=CARTESIAN_POINT('Origin',(1.2,-11.,19.));
#11613=CARTESIAN_POINT('',(2.,-11.,19.275));
#11614=CARTESIAN_POINT('',(1.1,-11.,19.275));
#11615=CARTESIAN_POINT('Origin',(2.,-11.,19.));
#11616=CARTESIAN_POINT('Origin',(-1.,-9.,18.6));
#11617=CARTESIAN_POINT('',(1.2,-8.,18.6));
#11618=CARTESIAN_POINT('',(1.2,-9.,18.6));
#11619=CARTESIAN_POINT('',(1.2,-8.5,18.6));
#11620=CARTESIAN_POINT('',(-1.,-8.,18.6));
#11621=CARTESIAN_POINT('',(2.,-8.,18.6));
#11622=CARTESIAN_POINT('',(-1.,-9.,18.6));
#11623=CARTESIAN_POINT('',(-1.,-9.,18.6));
#11624=CARTESIAN_POINT('',(2.,-9.,18.6));
#11625=CARTESIAN_POINT('Origin',(-1.,-9.,18.));
#11626=CARTESIAN_POINT('',(-1.,-9.,18.));
#11627=CARTESIAN_POINT('',(-1.,-9.,18.6));
#11628=CARTESIAN_POINT('',(-1.,-8.,18.));
#11629=CARTESIAN_POINT('',(-1.,-8.,18.6));
#11630=CARTESIAN_POINT('',(-1.,-9.,18.));
#11631=CARTESIAN_POINT('Origin',(0.5,-9.,18.3));
#11632=CARTESIAN_POINT('',(1.2,-9.,18.));
#11633=CARTESIAN_POINT('',(1.2,-9.,18.15));
#11634=CARTESIAN_POINT('',(-1.,-9.,18.));
#11635=CARTESIAN_POINT('Origin',(2.,-8.,18.));
#11636=CARTESIAN_POINT('',(1.2,-8.,20.));
#11637=CARTESIAN_POINT('',(1.2,-8.,18.));
#11638=CARTESIAN_POINT('',(2.,-8.,20.));
#11639=CARTESIAN_POINT('',(2.,-8.,20.));
#11640=CARTESIAN_POINT('',(2.,-8.,18.));
#11641=CARTESIAN_POINT('',(2.,-8.,18.));
#11642=CARTESIAN_POINT('',(2.,-8.,18.));
#11643=CARTESIAN_POINT('Origin',(1.6,-10.,18.));
#11644=CARTESIAN_POINT('',(2.,-12.,18.));
#11645=CARTESIAN_POINT('',(2.,-12.,18.));
#11646=CARTESIAN_POINT('',(1.2,-12.,18.));
#11647=CARTESIAN_POINT('',(1.2,-12.,18.));
#11648=CARTESIAN_POINT('',(1.2,-8.,18.));
#11649=CARTESIAN_POINT('Origin',(2.,-12.,18.));
#11650=CARTESIAN_POINT('',(2.,-12.,20.));
#11651=CARTESIAN_POINT('',(2.,-12.,20.));
#11652=CARTESIAN_POINT('',(2.,-12.,18.));
#11653=CARTESIAN_POINT('Origin',(1.2,-12.,18.));
#11654=CARTESIAN_POINT('',(1.2,-12.,20.));
#11655=CARTESIAN_POINT('',(1.2,-12.,20.));
#11656=CARTESIAN_POINT('',(1.2,-12.,18.));
#11657=CARTESIAN_POINT('Origin',(1.2,-8.,18.));
#11658=CARTESIAN_POINT('',(1.2,-8.,20.));
#11659=CARTESIAN_POINT('Origin',(1.6,-10.,20.));
#11660=CARTESIAN_POINT('',(0.,0.,0.));
#11661=CARTESIAN_POINT('Origin',(-1.1,-8.4,30.3));
#11662=CARTESIAN_POINT('',(-1.,-8.4,30.465));
#11663=CARTESIAN_POINT('Origin',(-1.,-8.4,30.3));
#11664=CARTESIAN_POINT('',(0.4,-8.4,30.465));
#11665=CARTESIAN_POINT('',(-1.1,-8.4,30.465));
#11666=CARTESIAN_POINT('Origin',(0.4,-8.4,30.3));
#11667=CARTESIAN_POINT('Origin',(0.4,-8.4,30.3));
#11668=CARTESIAN_POINT('Origin',(1.1,-11.,31.));
#11669=CARTESIAN_POINT('',(1.2,-11.,31.275));
#11670=CARTESIAN_POINT('Origin',(1.2,-11.,31.));
#11671=CARTESIAN_POINT('',(2.,-11.,31.275));
#11672=CARTESIAN_POINT('',(1.1,-11.,31.275));
#11673=CARTESIAN_POINT('Origin',(2.,-11.,31.));
#11674=CARTESIAN_POINT('Origin',(-1.,-9.,30.6));
#11675=CARTESIAN_POINT('',(1.2,-8.,30.6));
#11676=CARTESIAN_POINT('',(1.2,-9.,30.6));
#11677=CARTESIAN_POINT('',(1.2,-8.5,30.6));
#11678=CARTESIAN_POINT('',(-1.,-8.,30.6));
#11679=CARTESIAN_POINT('',(2.,-8.,30.6));
#11680=CARTESIAN_POINT('',(-1.,-9.,30.6));
#11681=CARTESIAN_POINT('',(-1.,-9.,30.6));
#11682=CARTESIAN_POINT('',(2.,-9.,30.6));
#11683=CARTESIAN_POINT('Origin',(-1.,-9.,30.));
#11684=CARTESIAN_POINT('',(-1.,-9.,30.));
#11685=CARTESIAN_POINT('',(-1.,-9.,30.6));
#11686=CARTESIAN_POINT('',(-1.,-8.,30.));
#11687=CARTESIAN_POINT('',(-1.,-8.,30.6));
#11688=CARTESIAN_POINT('',(-1.,-9.,30.));
#11689=CARTESIAN_POINT('Origin',(0.5,-9.,30.3));
#11690=CARTESIAN_POINT('',(1.2,-9.,30.));
#11691=CARTESIAN_POINT('',(1.2,-9.,30.15));
#11692=CARTESIAN_POINT('',(-1.,-9.,30.));
#11693=CARTESIAN_POINT('Origin',(2.,-8.,30.));
#11694=CARTESIAN_POINT('',(1.2,-8.,32.));
#11695=CARTESIAN_POINT('',(1.2,-8.,30.));
#11696=CARTESIAN_POINT('',(2.,-8.,32.));
#11697=CARTESIAN_POINT('',(2.,-8.,32.));
#11698=CARTESIAN_POINT('',(2.,-8.,30.));
#11699=CARTESIAN_POINT('',(2.,-8.,30.));
#11700=CARTESIAN_POINT('',(2.,-8.,30.));
#11701=CARTESIAN_POINT('Origin',(1.6,-10.,30.));
#11702=CARTESIAN_POINT('',(2.,-12.,30.));
#11703=CARTESIAN_POINT('',(2.,-12.,30.));
#11704=CARTESIAN_POINT('',(1.2,-12.,30.));
#11705=CARTESIAN_POINT('',(1.2,-12.,30.));
#11706=CARTESIAN_POINT('',(1.2,-8.,30.));
#11707=CARTESIAN_POINT('Origin',(2.,-12.,30.));
#11708=CARTESIAN_POINT('',(2.,-12.,32.));
#11709=CARTESIAN_POINT('',(2.,-12.,32.));
#11710=CARTESIAN_POINT('',(2.,-12.,30.));
#11711=CARTESIAN_POINT('Origin',(1.2,-12.,30.));
#11712=CARTESIAN_POINT('',(1.2,-12.,32.));
#11713=CARTESIAN_POINT('',(1.2,-12.,32.));
#11714=CARTESIAN_POINT('',(1.2,-12.,30.));
#11715=CARTESIAN_POINT('Origin',(1.2,-8.,30.));
#11716=CARTESIAN_POINT('',(1.2,-8.,32.));
#11717=CARTESIAN_POINT('Origin',(1.6,-10.,32.));
#11718=CARTESIAN_POINT('',(0.,0.,0.));
#11719=CARTESIAN_POINT('Origin',(-1.5,11.,6.95));
#11720=CARTESIAN_POINT('',(-1.4,11.,7.225));
#11721=CARTESIAN_POINT('Origin',(-1.4,11.,6.95));
#11722=CARTESIAN_POINT('',(1.2,11.,7.225));
#11723=CARTESIAN_POINT('',(-1.5,11.,7.225));
#11724=CARTESIAN_POINT('Origin',(1.2,11.,6.95));
#11725=CARTESIAN_POINT('Origin',(1.2,12.,6.6));
#11726=CARTESIAN_POINT('',(1.2,12.,6.6));
#11727=CARTESIAN_POINT('',(-1.4,12.,6.6));
#11728=CARTESIAN_POINT('',(1.2,12.,6.6));
#11729=CARTESIAN_POINT('',(-1.4,12.,7.3));
#11730=CARTESIAN_POINT('',(-1.4,12.,6.6));
#11731=CARTESIAN_POINT('',(1.2,12.,7.3));
#11732=CARTESIAN_POINT('',(1.2,12.,7.3));
#11733=CARTESIAN_POINT('',(1.2,12.,6.6));
#11734=CARTESIAN_POINT('Origin',(1.2,10.,6.6));
#11735=CARTESIAN_POINT('',(1.2,10.,6.6));
#11736=CARTESIAN_POINT('',(1.2,10.,6.6));
#11737=CARTESIAN_POINT('',(1.2,10.,7.3));
#11738=CARTESIAN_POINT('',(1.2,10.,7.3));
#11739=CARTESIAN_POINT('',(1.2,10.,6.6));
#11740=CARTESIAN_POINT('Origin',(-1.4,10.,6.6));
#11741=CARTESIAN_POINT('',(-1.4,10.,6.6));
#11742=CARTESIAN_POINT('',(-1.4,10.,6.6));
#11743=CARTESIAN_POINT('',(-1.4,10.,7.3));
#11744=CARTESIAN_POINT('',(-1.4,10.,7.3));
#11745=CARTESIAN_POINT('',(-1.4,10.,6.6));
#11746=CARTESIAN_POINT('Origin',(-1.4,12.,6.6));
#11747=CARTESIAN_POINT('',(-1.4,12.,6.6));
#11748=CARTESIAN_POINT('',(-1.4,12.,7.3));
#11749=CARTESIAN_POINT('Origin',(-0.1,11.,7.3));
#11750=CARTESIAN_POINT('Origin',(-0.1,11.,6.6));
#11751=CARTESIAN_POINT('',(0.,0.,0.));
#11752=CARTESIAN_POINT('Origin',(-1.5,11.,30.25));
#11753=CARTESIAN_POINT('',(-1.4,11.,30.525));
#11754=CARTESIAN_POINT('Origin',(-1.4,11.,30.25));
#11755=CARTESIAN_POINT('',(1.2,11.,30.525));
#11756=CARTESIAN_POINT('',(-1.5,11.,30.525));
#11757=CARTESIAN_POINT('Origin',(1.2,11.,30.25));
#11758=CARTESIAN_POINT('Origin',(1.2,12.,29.9));
#11759=CARTESIAN_POINT('',(1.2,12.,29.9));
#11760=CARTESIAN_POINT('',(-1.4,12.,29.9));
#11761=CARTESIAN_POINT('',(1.2,12.,29.9));
#11762=CARTESIAN_POINT('',(-1.4,12.,30.6));
#11763=CARTESIAN_POINT('',(-1.4,12.,29.9));
#11764=CARTESIAN_POINT('',(1.2,12.,30.6));
#11765=CARTESIAN_POINT('',(1.2,12.,30.6));
#11766=CARTESIAN_POINT('',(1.2,12.,29.9));
#11767=CARTESIAN_POINT('Origin',(1.2,10.,29.9));
#11768=CARTESIAN_POINT('',(1.2,10.,29.9));
#11769=CARTESIAN_POINT('',(1.2,10.,29.9));
#11770=CARTESIAN_POINT('',(1.2,10.,30.6));
#11771=CARTESIAN_POINT('',(1.2,10.,30.6));
#11772=CARTESIAN_POINT('',(1.2,10.,29.9));
#11773=CARTESIAN_POINT('Origin',(-1.4,10.,29.9));
#11774=CARTESIAN_POINT('',(-1.4,10.,29.9));
#11775=CARTESIAN_POINT('',(-1.4,10.,29.9));
#11776=CARTESIAN_POINT('',(-1.4,10.,30.6));
#11777=CARTESIAN_POINT('',(-1.4,10.,30.6));
#11778=CARTESIAN_POINT('',(-1.4,10.,29.9));
#11779=CARTESIAN_POINT('Origin',(-1.4,12.,29.9));
#11780=CARTESIAN_POINT('',(-1.4,12.,29.9));
#11781=CARTESIAN_POINT('',(-1.4,12.,30.6));
#11782=CARTESIAN_POINT('Origin',(-0.1,11.,30.6));
#11783=CARTESIAN_POINT('Origin',(-0.1,11.,29.9));
#11784=CARTESIAN_POINT('',(0.,0.,0.));
#11785=CARTESIAN_POINT('Origin',(-0.1,0.82,-0.3));
#11786=CARTESIAN_POINT('',(0.,0.82,-0.3));
#11787=CARTESIAN_POINT('',(0.,1.,-0.3));
#11788=CARTESIAN_POINT('',(0.,0.41,-0.3));
#11789=CARTESIAN_POINT('',(40.,0.82,-0.3));
#11790=CARTESIAN_POINT('',(-0.1,0.82,-0.3));
#11791=CARTESIAN_POINT('',(40.,1.,-0.3));
#11792=CARTESIAN_POINT('',(40.,0.41,-0.3));
#11793=CARTESIAN_POINT('',(-0.05,1.,-0.3));
#11794=CARTESIAN_POINT('Origin',(-0.1,0.82,-0.55));
#11795=CARTESIAN_POINT('',(0.,0.82,-0.55));
#11796=CARTESIAN_POINT('',(0.,0.82,-0.275));
#11797=CARTESIAN_POINT('',(40.,0.82,-0.55));
#11798=CARTESIAN_POINT('',(-0.1,0.82,-0.55));
#11799=CARTESIAN_POINT('',(40.,0.82,-0.275));
#11800=CARTESIAN_POINT('Origin',(-0.1,0.67,-0.55));
#11801=CARTESIAN_POINT('',(0.,0.67,-0.55));
#11802=CARTESIAN_POINT('',(0.,0.335,-0.55));
#11803=CARTESIAN_POINT('',(40.,0.67,-0.55));
#11804=CARTESIAN_POINT('',(-0.1,0.67,-0.55));
#11805=CARTESIAN_POINT('',(40.,0.335,-0.55));
#11806=CARTESIAN_POINT('Origin',(-0.1,0.42,-0.3));
#11807=CARTESIAN_POINT('',(0.,0.42,-0.3));
#11808=CARTESIAN_POINT('',(0.,0.24,-0.12));
#11809=CARTESIAN_POINT('',(40.,0.42,-0.3));
#11810=CARTESIAN_POINT('',(-0.1,0.42,-0.3));
#11811=CARTESIAN_POINT('',(40.,0.24,-0.12));
#11812=CARTESIAN_POINT('Origin',(-0.1,0.42,0.3));
#11813=CARTESIAN_POINT('',(0.,0.42,0.3));
#11814=CARTESIAN_POINT('',(0.,0.42,0.15));
#11815=CARTESIAN_POINT('',(40.,0.42,0.3));
#11816=CARTESIAN_POINT('',(-0.1,0.42,0.3));
#11817=CARTESIAN_POINT('',(40.,0.42,0.15));
#11818=CARTESIAN_POINT('Origin',(-0.1,0.67,0.55));
#11819=CARTESIAN_POINT('',(0.,0.67,0.55));
#11820=CARTESIAN_POINT('',(6.93889390390723E-18,0.365,0.245));
#11821=CARTESIAN_POINT('',(40.,0.67,0.55));
#11822=CARTESIAN_POINT('',(-0.1,0.67,0.55));
#11823=CARTESIAN_POINT('',(40.,0.365,0.245));
#11824=CARTESIAN_POINT('Origin',(-0.1,0.82,0.55));
#11825=CARTESIAN_POINT('',(0.,0.82,0.55));
#11826=CARTESIAN_POINT('',(0.,0.41,0.55));
#11827=CARTESIAN_POINT('',(40.,0.82,0.55));
#11828=CARTESIAN_POINT('',(-0.1,0.82,0.55));
#11829=CARTESIAN_POINT('',(40.,0.41,0.55));
#11830=CARTESIAN_POINT('Origin',(-0.1,0.82,0.3));
#11831=CARTESIAN_POINT('',(0.,0.82,0.3));
#11832=CARTESIAN_POINT('',(0.,0.82,0.15));
#11833=CARTESIAN_POINT('',(40.,0.82,0.3));
#11834=CARTESIAN_POINT('',(-0.1,0.82,0.3));
#11835=CARTESIAN_POINT('',(40.,0.82,0.15));
#11836=CARTESIAN_POINT('Origin',(-0.1,1.05,0.3));
#11837=CARTESIAN_POINT('',(0.,1.,0.3));
#11838=CARTESIAN_POINT('',(0.,0.525,0.3));
#11839=CARTESIAN_POINT('',(40.,1.,0.3));
#11840=CARTESIAN_POINT('',(-0.05,1.,0.3));
#11841=CARTESIAN_POINT('',(40.,0.525,0.3));
#11842=CARTESIAN_POINT('Origin',(-0.1,-0.3,-0.82));
#11843=CARTESIAN_POINT('',(0.,-0.3,-0.82));
#11844=CARTESIAN_POINT('',(0.,-0.3,-1.));
#11845=CARTESIAN_POINT('',(0.,-0.3,-0.41));
#11846=CARTESIAN_POINT('',(40.,-0.3,-0.82));
#11847=CARTESIAN_POINT('',(-0.1,-0.3,-0.82));
#11848=CARTESIAN_POINT('',(40.,-0.3,-1.));
#11849=CARTESIAN_POINT('',(40.,-0.3,-0.41));
#11850=CARTESIAN_POINT('',(-0.05,-0.3,-1.));
#11851=CARTESIAN_POINT('Origin',(-0.1,-0.55,-0.82));
#11852=CARTESIAN_POINT('',(0.,-0.55,-0.82));
#11853=CARTESIAN_POINT('',(0.,-0.275,-0.82));
#11854=CARTESIAN_POINT('',(40.,-0.55,-0.82));
#11855=CARTESIAN_POINT('',(-0.1,-0.55,-0.82));
#11856=CARTESIAN_POINT('',(40.,-0.275,-0.82));
#11857=CARTESIAN_POINT('Origin',(-0.1,-0.55,-0.67));
#11858=CARTESIAN_POINT('',(0.,-0.55,-0.67));
#11859=CARTESIAN_POINT('',(0.,-0.55,-0.335));
#11860=CARTESIAN_POINT('',(40.,-0.55,-0.67));
#11861=CARTESIAN_POINT('',(-0.1,-0.55,-0.67));
#11862=CARTESIAN_POINT('',(40.,-0.55,-0.335));
#11863=CARTESIAN_POINT('Origin',(-0.1,-0.3,-0.42));
#11864=CARTESIAN_POINT('',(0.,-0.3,-0.42));
#11865=CARTESIAN_POINT('',(0.,-0.12,-0.24));
#11866=CARTESIAN_POINT('',(40.,-0.3,-0.42));
#11867=CARTESIAN_POINT('',(-0.1,-0.3,-0.42));
#11868=CARTESIAN_POINT('',(40.,-0.12,-0.24));
#11869=CARTESIAN_POINT('Origin',(-0.1,0.3,-0.42));
#11870=CARTESIAN_POINT('',(0.,0.3,-0.42));
#11871=CARTESIAN_POINT('',(0.,0.15,-0.42));
#11872=CARTESIAN_POINT('',(40.,0.3,-0.42));
#11873=CARTESIAN_POINT('',(-0.1,0.3,-0.42));
#11874=CARTESIAN_POINT('',(40.,0.15,-0.42));
#11875=CARTESIAN_POINT('Origin',(-0.1,0.55,-0.67));
#11876=CARTESIAN_POINT('',(0.,0.55,-0.67));
#11877=CARTESIAN_POINT('',(0.,0.245,-0.365));
#11878=CARTESIAN_POINT('',(40.,0.55,-0.67));
#11879=CARTESIAN_POINT('',(-0.1,0.55,-0.67));
#11880=CARTESIAN_POINT('',(40.,0.245,-0.365));
#11881=CARTESIAN_POINT('Origin',(-0.1,0.55,-0.82));
#11882=CARTESIAN_POINT('',(0.,0.55,-0.82));
#11883=CARTESIAN_POINT('',(0.,0.55,-0.41));
#11884=CARTESIAN_POINT('',(40.,0.55,-0.82));
#11885=CARTESIAN_POINT('',(-0.1,0.55,-0.82));
#11886=CARTESIAN_POINT('',(40.,0.55,-0.41));
#11887=CARTESIAN_POINT('Origin',(-0.1,0.3,-0.82));
#11888=CARTESIAN_POINT('',(0.,0.3,-0.82));
#11889=CARTESIAN_POINT('',(0.,0.15,-0.82));
#11890=CARTESIAN_POINT('',(40.,0.3,-0.82));
#11891=CARTESIAN_POINT('',(-0.1,0.3,-0.82));
#11892=CARTESIAN_POINT('',(40.,0.15,-0.82));
#11893=CARTESIAN_POINT('Origin',(-0.1,0.3,-1.05));
#11894=CARTESIAN_POINT('',(0.,0.3,-1.));
#11895=CARTESIAN_POINT('',(0.,0.3,-0.525));
#11896=CARTESIAN_POINT('',(40.,0.3,-1.));
#11897=CARTESIAN_POINT('',(-0.05,0.3,-1.));
#11898=CARTESIAN_POINT('',(40.,0.3,-0.525));
#11899=CARTESIAN_POINT('Origin',(-0.1,-0.82,0.3));
#11900=CARTESIAN_POINT('',(0.,-0.82,0.3));
#11901=CARTESIAN_POINT('',(0.,-1.,0.3));
#11902=CARTESIAN_POINT('',(0.,-0.41,0.3));
#11903=CARTESIAN_POINT('',(40.,-0.82,0.3));
#11904=CARTESIAN_POINT('',(-0.1,-0.82,0.3));
#11905=CARTESIAN_POINT('',(40.,-1.,0.3));
#11906=CARTESIAN_POINT('',(40.,-0.41,0.3));
#11907=CARTESIAN_POINT('',(-0.05,-1.,0.3));
#11908=CARTESIAN_POINT('Origin',(-0.1,-0.82,0.55));
#11909=CARTESIAN_POINT('',(0.,-0.82,0.55));
#11910=CARTESIAN_POINT('',(0.,-0.82,0.275));
#11911=CARTESIAN_POINT('',(40.,-0.82,0.55));
#11912=CARTESIAN_POINT('',(-0.1,-0.82,0.55));
#11913=CARTESIAN_POINT('',(40.,-0.82,0.275));
#11914=CARTESIAN_POINT('Origin',(-0.1,-0.67,0.55));
#11915=CARTESIAN_POINT('',(0.,-0.67,0.55));
#11916=CARTESIAN_POINT('',(0.,-0.335,0.55));
#11917=CARTESIAN_POINT('',(40.,-0.67,0.55));
#11918=CARTESIAN_POINT('',(-0.1,-0.67,0.55));
#11919=CARTESIAN_POINT('',(40.,-0.335,0.55));
#11920=CARTESIAN_POINT('Origin',(-0.1,-0.42,0.3));
#11921=CARTESIAN_POINT('',(0.,-0.42,0.3));
#11922=CARTESIAN_POINT('',(-6.93889390390723E-18,-0.24,0.12));
#11923=CARTESIAN_POINT('',(40.,-0.42,0.3));
#11924=CARTESIAN_POINT('',(-0.1,-0.42,0.3));
#11925=CARTESIAN_POINT('',(40.,-0.24,0.12));
#11926=CARTESIAN_POINT('Origin',(-0.1,-0.42,-0.3));
#11927=CARTESIAN_POINT('',(0.,-0.42,-0.3));
#11928=CARTESIAN_POINT('',(0.,-0.42,-0.15));
#11929=CARTESIAN_POINT('',(40.,-0.42,-0.3));
#11930=CARTESIAN_POINT('',(-0.1,-0.42,-0.3));
#11931=CARTESIAN_POINT('',(40.,-0.42,-0.15));
#11932=CARTESIAN_POINT('Origin',(-0.1,-0.67,-0.55));
#11933=CARTESIAN_POINT('',(0.,-0.67,-0.55));
#11934=CARTESIAN_POINT('',(0.,-0.365,-0.245));
#11935=CARTESIAN_POINT('',(40.,-0.67,-0.55));
#11936=CARTESIAN_POINT('',(-0.1,-0.67,-0.55));
#11937=CARTESIAN_POINT('',(40.,-0.365,-0.245));
#11938=CARTESIAN_POINT('Origin',(-0.1,-0.82,-0.55));
#11939=CARTESIAN_POINT('',(0.,-0.82,-0.55));
#11940=CARTESIAN_POINT('',(0.,-0.41,-0.55));
#11941=CARTESIAN_POINT('',(40.,-0.82,-0.55));
#11942=CARTESIAN_POINT('',(-0.1,-0.82,-0.55));
#11943=CARTESIAN_POINT('',(40.,-0.41,-0.55));
#11944=CARTESIAN_POINT('Origin',(-0.1,-0.82,-0.3));
#11945=CARTESIAN_POINT('',(0.,-0.82,-0.3));
#11946=CARTESIAN_POINT('',(0.,-0.82,-0.15));
#11947=CARTESIAN_POINT('',(40.,-0.82,-0.3));
#11948=CARTESIAN_POINT('',(-0.1,-0.82,-0.3));
#11949=CARTESIAN_POINT('',(40.,-0.82,-0.15));
#11950=CARTESIAN_POINT('Origin',(-0.1,-1.05,-0.3));
#11951=CARTESIAN_POINT('',(0.,-1.,-0.3));
#11952=CARTESIAN_POINT('',(0.,-0.525,-0.3));
#11953=CARTESIAN_POINT('',(40.,-1.,-0.3));
#11954=CARTESIAN_POINT('',(-0.05,-1.,-0.3));
#11955=CARTESIAN_POINT('',(40.,-0.525,-0.3));
#11956=CARTESIAN_POINT('Origin',(-0.1,0.3,0.82));
#11957=CARTESIAN_POINT('',(0.,0.3,0.82));
#11958=CARTESIAN_POINT('',(0.,0.3,1.));
#11959=CARTESIAN_POINT('',(0.,0.3,0.41));
#11960=CARTESIAN_POINT('',(40.,0.3,0.82));
#11961=CARTESIAN_POINT('',(-0.1,0.3,0.82));
#11962=CARTESIAN_POINT('',(40.,0.3,1.));
#11963=CARTESIAN_POINT('',(40.,0.3,0.41));
#11964=CARTESIAN_POINT('',(-0.05,0.3,1.));
#11965=CARTESIAN_POINT('Origin',(-0.1,0.55,0.82));
#11966=CARTESIAN_POINT('',(0.,0.55,0.82));
#11967=CARTESIAN_POINT('',(0.,0.275,0.82));
#11968=CARTESIAN_POINT('',(40.,0.55,0.82));
#11969=CARTESIAN_POINT('',(-0.1,0.55,0.82));
#11970=CARTESIAN_POINT('',(40.,0.275,0.82));
#11971=CARTESIAN_POINT('Origin',(-0.1,0.55,0.67));
#11972=CARTESIAN_POINT('',(0.,0.55,0.67));
#11973=CARTESIAN_POINT('',(0.,0.55,0.335));
#11974=CARTESIAN_POINT('',(40.,0.55,0.67));
#11975=CARTESIAN_POINT('',(-0.1,0.55,0.67));
#11976=CARTESIAN_POINT('',(40.,0.55,0.335));
#11977=CARTESIAN_POINT('Origin',(-0.1,0.3,0.42));
#11978=CARTESIAN_POINT('',(0.,0.3,0.42));
#11979=CARTESIAN_POINT('',(6.93889390390723E-18,0.12,0.24));
#11980=CARTESIAN_POINT('',(40.,0.3,0.42));
#11981=CARTESIAN_POINT('',(-0.1,0.3,0.42));
#11982=CARTESIAN_POINT('',(40.,0.12,0.24));
#11983=CARTESIAN_POINT('Origin',(-0.1,-0.3,0.42));
#11984=CARTESIAN_POINT('',(0.,-0.3,0.42));
#11985=CARTESIAN_POINT('',(0.,-0.15,0.42));
#11986=CARTESIAN_POINT('',(40.,-0.3,0.42));
#11987=CARTESIAN_POINT('',(-0.1,-0.3,0.42));
#11988=CARTESIAN_POINT('',(40.,-0.15,0.42));
#11989=CARTESIAN_POINT('Origin',(-0.1,-0.55,0.67));
#11990=CARTESIAN_POINT('',(0.,-0.55,0.67));
#11991=CARTESIAN_POINT('',(6.93889390390723E-18,-0.245,0.365));
#11992=CARTESIAN_POINT('',(40.,-0.55,0.67));
#11993=CARTESIAN_POINT('',(-0.1,-0.55,0.67));
#11994=CARTESIAN_POINT('',(40.,-0.245,0.365));
#11995=CARTESIAN_POINT('Origin',(-0.1,-0.55,0.82));
#11996=CARTESIAN_POINT('',(0.,-0.55,0.82));
#11997=CARTESIAN_POINT('',(0.,-0.55,0.41));
#11998=CARTESIAN_POINT('',(40.,-0.55,0.82));
#11999=CARTESIAN_POINT('',(-0.1,-0.55,0.82));
#12000=CARTESIAN_POINT('',(40.,-0.55,0.41));
#12001=CARTESIAN_POINT('Origin',(-0.1,-0.3,0.82));
#12002=CARTESIAN_POINT('',(0.,-0.3,0.82));
#12003=CARTESIAN_POINT('',(0.,-0.15,0.82));
#12004=CARTESIAN_POINT('',(40.,-0.3,0.82));
#12005=CARTESIAN_POINT('',(-0.1,-0.3,0.82));
#12006=CARTESIAN_POINT('',(40.,-0.15,0.82));
#12007=CARTESIAN_POINT('Origin',(-0.1,-0.3,1.05));
#12008=CARTESIAN_POINT('',(0.,-0.3,1.));
#12009=CARTESIAN_POINT('',(0.,-0.3,0.525));
#12010=CARTESIAN_POINT('',(40.,-0.3,1.));
#12011=CARTESIAN_POINT('',(-0.05,-0.3,1.));
#12012=CARTESIAN_POINT('',(40.,-0.3,0.525));
#12013=CARTESIAN_POINT('Origin',(-0.1,0.,0.));
#12014=CARTESIAN_POINT('',(0.,-2.57175827820944E-17,0.21));
#12015=CARTESIAN_POINT('Origin',(0.,0.,0.));
#12016=CARTESIAN_POINT('',(40.,2.57175827820944E-17,0.21));
#12017=CARTESIAN_POINT('',(-0.1,-2.57175827820944E-17,0.21));
#12018=CARTESIAN_POINT('Origin',(40.,0.,0.));
#12019=CARTESIAN_POINT('Origin',(0.,1.,-1.));
#12020=CARTESIAN_POINT('',(0.,1.,1.));
#12021=CARTESIAN_POINT('',(0.,1.,-1.));
#12022=CARTESIAN_POINT('',(40.,1.,1.));
#12023=CARTESIAN_POINT('',(0.,1.,1.));
#12024=CARTESIAN_POINT('',(40.,1.,-1.));
#12025=CARTESIAN_POINT('Origin',(0.,1.,-1.));
#12026=CARTESIAN_POINT('',(40.,1.,-1.));
#12027=CARTESIAN_POINT('',(40.,1.,-1.));
#12028=CARTESIAN_POINT('',(0.,1.,-1.));
#12029=CARTESIAN_POINT('',(0.,1.,-1.));
#12030=CARTESIAN_POINT('',(0.,1.,-1.));
#12031=CARTESIAN_POINT('Origin',(0.,-1.,-1.));
#12032=CARTESIAN_POINT('',(0.,-1.,-1.));
#12033=CARTESIAN_POINT('',(40.,-1.,-1.));
#12034=CARTESIAN_POINT('Origin',(0.,-1.,-1.));
#12035=CARTESIAN_POINT('',(40.,-1.,-1.));
#12036=CARTESIAN_POINT('',(40.,-1.,-1.));
#12037=CARTESIAN_POINT('',(0.,-1.,-1.));
#12038=CARTESIAN_POINT('',(0.,-1.,-1.));
#12039=CARTESIAN_POINT('',(0.,-1.,-1.));
#12040=CARTESIAN_POINT('Origin',(0.,-1.,1.));
#12041=CARTESIAN_POINT('',(0.,-1.,1.));
#12042=CARTESIAN_POINT('',(40.,-1.,1.));
#12043=CARTESIAN_POINT('Origin',(0.,-1.,1.));
#12044=CARTESIAN_POINT('',(40.,-1.,1.));
#12045=CARTESIAN_POINT('',(40.,-1.,1.));
#12046=CARTESIAN_POINT('',(0.,-1.,1.));
#12047=CARTESIAN_POINT('',(0.,-1.,1.));
#12048=CARTESIAN_POINT('',(0.,-1.,1.));
#12049=CARTESIAN_POINT('Origin',(0.,1.,1.));
#12050=CARTESIAN_POINT('',(0.,1.,1.));
#12051=CARTESIAN_POINT('',(40.,1.,1.));
#12052=CARTESIAN_POINT('Origin',(0.,1.,1.));
#12053=CARTESIAN_POINT('',(40.,1.,1.));
#12054=CARTESIAN_POINT('',(0.,1.,1.));
#12055=CARTESIAN_POINT('Origin',(40.,0.,0.));
#12056=CARTESIAN_POINT('Origin',(0.,0.,0.));
#12057=CARTESIAN_POINT('',(0.,0.,0.));
#12058=CARTESIAN_POINT('Origin',(0.375,0.5,0.));
#12059=CARTESIAN_POINT('',(-0.375,0.5,-4.59242549680257E-17));
#12060=CARTESIAN_POINT('Origin',(0.,0.5,0.));
#12061=CARTESIAN_POINT('Origin',(0.,0.475,0.));
#12062=CARTESIAN_POINT('',(-0.425,0.45,-5.20474889637625E-17));
#12063=CARTESIAN_POINT('Origin',(0.,0.45,0.));
#12064=CARTESIAN_POINT('',(-0.4,0.475,-4.89858719658941E-17));
#12065=CARTESIAN_POINT('Origin',(0.,0.24,0.));
#12066=CARTESIAN_POINT('',(-0.425,0.0299999999999998,-5.20474889637625E-17));
#12067=CARTESIAN_POINT('Origin',(0.,0.0299999999999998,0.));
#12068=CARTESIAN_POINT('',(-0.425,0.24,-5.20474889637625E-17));
#12069=CARTESIAN_POINT('Origin',(0.,0.0150000000000001,0.));
#12070=CARTESIAN_POINT('',(-0.395,4.85722573273506E-17,-4.83735485663204E-17));
#12071=CARTESIAN_POINT('Origin',(0.,0.,0.));
#12072=CARTESIAN_POINT('',(-0.41,0.0150000000000001,-5.02105187650415E-17));
#12073=CARTESIAN_POINT('Origin',(0.27,0.,0.));
#12074=CARTESIAN_POINT('',(-0.27,0.,-3.30654635769785E-17));
#12075=CARTESIAN_POINT('Origin',(0.,0.,0.));
#12076=CARTESIAN_POINT('Origin',(0.,-0.02,0.));
#12077=CARTESIAN_POINT('',(-0.24505,-0.0498999999999999,3.00099698131059E-17));
#12078=CARTESIAN_POINT('Origin',(0.,-0.0498999999999999,0.));
#12079=CARTESIAN_POINT('',(-0.26,-0.02,-3.18408167778312E-17));
#12080=CARTESIAN_POINT('Origin',(0.,-0.995,0.));
#12081=CARTESIAN_POINT('',(-0.24505,-1.95495,3.00099698131059E-17));
#12082=CARTESIAN_POINT('Origin',(0.,-1.95495,0.));
#12083=CARTESIAN_POINT('',(-0.24505,-0.995,-3.00099698131059E-17));
#12084=CARTESIAN_POINT('Origin',(0.,-1.975,0.));
#12085=CARTESIAN_POINT('',(-0.2,-2.,-2.44929359829471E-17));
#12086=CARTESIAN_POINT('Origin',(0.,-2.,0.));
#12087=CARTESIAN_POINT('',(-0.225,-1.975,-2.75545529808154E-17));
#12088=CARTESIAN_POINT('Origin',(0.,-2.,0.));
#12089=CARTESIAN_POINT('Origin',(0.115470053837925,-0.5,-0.2));
#12090=CARTESIAN_POINT('',(0.23094010767585,-0.5,0.));
#12091=CARTESIAN_POINT('',(0.115470053837925,-0.5,-0.2));
#12092=CARTESIAN_POINT('',(0.23094010767585,-0.5,0.));
#12093=CARTESIAN_POINT('',(0.115470053837925,-0.8,-0.2));
#12094=CARTESIAN_POINT('',(0.115470053837925,-0.5,-0.2));
#12095=CARTESIAN_POINT('',(0.23094010767585,-0.8,0.));
#12096=CARTESIAN_POINT('',(0.23094010767585,-0.8,0.));
#12097=CARTESIAN_POINT('',(0.23094010767585,-0.5,0.));
#12098=CARTESIAN_POINT('Origin',(-0.115470053837925,-0.5,-0.2));
#12099=CARTESIAN_POINT('',(-0.115470053837925,-0.5,-0.2));
#12100=CARTESIAN_POINT('',(0.115470053837925,-0.5,-0.2));
#12101=CARTESIAN_POINT('',(-0.115470053837925,-0.8,-0.2));
#12102=CARTESIAN_POINT('',(-0.115470053837925,-0.5,-0.2));
#12103=CARTESIAN_POINT('',(0.115470053837925,-0.8,-0.2));
#12104=CARTESIAN_POINT('Origin',(-0.23094010767585,-0.5,-2.77555756156289E-17));
#12105=CARTESIAN_POINT('',(-0.23094010767585,-0.5,-2.82820063659975E-17));
#12106=CARTESIAN_POINT('',(-0.115470053837925,-0.5,-0.2));
#12107=CARTESIAN_POINT('',(-0.23094010767585,-0.8,-2.77555756156289E-17));
#12108=CARTESIAN_POINT('',(-0.23094010767585,-0.5,-2.82820063659975E-17));
#12109=CARTESIAN_POINT('',(-0.115470053837925,-0.8,-0.2));
#12110=CARTESIAN_POINT('Origin',(-0.115470053837925,-0.5,0.2));
#12111=CARTESIAN_POINT('',(-0.115470053837925,-0.5,0.2));
#12112=CARTESIAN_POINT('',(-0.23094010767585,-0.5,-2.82820063659975E-17));
#12113=CARTESIAN_POINT('',(-0.115470053837925,-0.8,0.2));
#12114=CARTESIAN_POINT('',(-0.115470053837925,-0.5,0.2));
#12115=CARTESIAN_POINT('',(-0.23094010767585,-0.8,-2.82820063659975E-17));
#12116=CARTESIAN_POINT('Origin',(0.115470053837925,-0.5,0.2));
#12117=CARTESIAN_POINT('',(0.115470053837925,-0.5,0.2));
#12118=CARTESIAN_POINT('',(-0.115470053837925,-0.5,0.2));
#12119=CARTESIAN_POINT('',(0.115470053837925,-0.8,0.2));
#12120=CARTESIAN_POINT('',(0.115470053837925,-0.5,0.2));
#12121=CARTESIAN_POINT('',(-0.115470053837925,-0.8,0.2));
#12122=CARTESIAN_POINT('Origin',(0.23094010767585,-0.5,0.));
#12123=CARTESIAN_POINT('',(0.115470053837925,-0.5,0.2));
#12124=CARTESIAN_POINT('',(0.115470053837925,-0.8,0.2));
#12125=CARTESIAN_POINT('Origin',(0.,-0.5,0.));
#12126=CARTESIAN_POINT('Origin',(0.,-0.8,0.));
#12127=CARTESIAN_POINT('',(0.,0.,0.));
#12128=CARTESIAN_POINT('Origin',(14.,0.,0.97));
#12129=CARTESIAN_POINT('',(13.625,-4.59242549680257E-17,0.97));
#12130=CARTESIAN_POINT('Origin',(14.,0.,0.97));
#12131=CARTESIAN_POINT('',(13.625,4.59242549680257E-17,1.5));
#12132=CARTESIAN_POINT('',(13.625,-4.59242549680257E-17,0.97));
#12133=CARTESIAN_POINT('Origin',(14.,0.,1.5));
#12134=CARTESIAN_POINT('Origin',(14.,0.,0.97));
#12135=CARTESIAN_POINT('',(13.775,-2.75545529808154E-17,0.97));
#12136=CARTESIAN_POINT('Origin',(14.,0.,0.97));
#12137=CARTESIAN_POINT('Origin',(8.,0.,0.97));
#12138=CARTESIAN_POINT('',(7.625,-4.59242549680257E-17,0.97));
#12139=CARTESIAN_POINT('Origin',(8.,0.,0.97));
#12140=CARTESIAN_POINT('',(7.625,4.59242549680257E-17,1.5));
#12141=CARTESIAN_POINT('',(7.625,-4.59242549680257E-17,0.97));
#12142=CARTESIAN_POINT('Origin',(8.,0.,1.5));
#12143=CARTESIAN_POINT('Origin',(8.,0.,0.97));
#12144=CARTESIAN_POINT('',(7.775,-2.75545529808154E-17,0.97));
#12145=CARTESIAN_POINT('Origin',(8.,0.,0.97));
#12146=CARTESIAN_POINT('Origin',(2.,0.,0.97));
#12147=CARTESIAN_POINT('',(1.625,-4.59242549680257E-17,0.97));
#12148=CARTESIAN_POINT('Origin',(2.,0.,0.97));
#12149=CARTESIAN_POINT('',(1.625,4.59242549680257E-17,1.5));
#12150=CARTESIAN_POINT('',(1.625,-4.59242549680257E-17,0.97));
#12151=CARTESIAN_POINT('Origin',(2.,0.,1.5));
#12152=CARTESIAN_POINT('Origin',(2.,0.,0.97));
#12153=CARTESIAN_POINT('',(1.775,-2.75545529808155E-17,0.97));
#12154=CARTESIAN_POINT('Origin',(2.,0.,0.97));
#12155=CARTESIAN_POINT('Origin',(20.,0.,0.97));
#12156=CARTESIAN_POINT('',(19.625,-4.59242549680257E-17,0.97));
#12157=CARTESIAN_POINT('Origin',(20.,0.,0.97));
#12158=CARTESIAN_POINT('',(19.625,4.59242549680257E-17,1.5));
#12159=CARTESIAN_POINT('',(19.625,-4.59242549680257E-17,0.97));
#12160=CARTESIAN_POINT('Origin',(20.,0.,1.5));
#12161=CARTESIAN_POINT('Origin',(20.,0.,0.97));
#12162=CARTESIAN_POINT('',(19.775,-2.75545529808156E-17,0.97));
#12163=CARTESIAN_POINT('Origin',(20.,0.,0.97));
#12164=CARTESIAN_POINT('Origin',(14.,0.,-0.1));
#12165=CARTESIAN_POINT('',(13.775,-2.75545529808154E-17,0.));
#12166=CARTESIAN_POINT('Origin',(14.,0.,0.));
#12167=CARTESIAN_POINT('',(13.775,-2.75545529808154E-17,-0.1));
#12168=CARTESIAN_POINT('Origin',(8.,0.,-0.1));
#12169=CARTESIAN_POINT('',(7.775,-2.75545529808154E-17,0.));
#12170=CARTESIAN_POINT('Origin',(8.,0.,0.));
#12171=CARTESIAN_POINT('',(7.775,-2.75545529808154E-17,-0.1));
#12172=CARTESIAN_POINT('Origin',(2.,0.,-0.1));
#12173=CARTESIAN_POINT('',(1.775,-2.75545529808155E-17,0.));
#12174=CARTESIAN_POINT('Origin',(2.,0.,0.));
#12175=CARTESIAN_POINT('',(1.775,-2.75545529808155E-17,-0.1));
#12176=CARTESIAN_POINT('Origin',(20.,0.,-0.1));
#12177=CARTESIAN_POINT('',(19.775,-2.75545529808156E-17,0.));
#12178=CARTESIAN_POINT('Origin',(20.,0.,0.));
#12179=CARTESIAN_POINT('',(19.775,-2.75545529808156E-17,-0.1));
#12180=CARTESIAN_POINT('Origin',(0.,-0.53,1.));
#12181=CARTESIAN_POINT('',(0.,-0.53,1.));
#12182=CARTESIAN_POINT('',(0.,-0.75,0.85));
#12183=CARTESIAN_POINT('',(0.,-0.53,1.));
#12184=CARTESIAN_POINT('',(22.,-0.75,0.85));
#12185=CARTESIAN_POINT('',(0.,-0.75,0.85));
#12186=CARTESIAN_POINT('',(22.,-0.53,1.));
#12187=CARTESIAN_POINT('',(22.,-0.53,1.));
#12188=CARTESIAN_POINT('',(0.,-0.53,1.));
#12189=CARTESIAN_POINT('Origin',(0.,-0.53,1.15));
#12190=CARTESIAN_POINT('',(0.,-0.53,1.15));
#12191=CARTESIAN_POINT('',(0.,-0.53,1.15));
#12192=CARTESIAN_POINT('',(22.,-0.53,1.15));
#12193=CARTESIAN_POINT('',(22.,-0.53,1.15));
#12194=CARTESIAN_POINT('',(0.,-0.53,1.15));
#12195=CARTESIAN_POINT('Origin',(0.,-0.75,1.3));
#12196=CARTESIAN_POINT('',(0.,-0.75,1.3));
#12197=CARTESIAN_POINT('',(0.,-0.75,1.3));
#12198=CARTESIAN_POINT('',(22.,-0.75,1.3));
#12199=CARTESIAN_POINT('',(22.,-0.75,1.3));
#12200=CARTESIAN_POINT('',(0.,-0.75,1.3));
#12201=CARTESIAN_POINT('Origin',(0.,-0.75,1.5));
#12202=CARTESIAN_POINT('',(0.,-0.75,1.5));
#12203=CARTESIAN_POINT('',(0.,-0.75,1.5));
#12204=CARTESIAN_POINT('',(22.,-0.75,1.5));
#12205=CARTESIAN_POINT('',(22.,-0.75,1.5));
#12206=CARTESIAN_POINT('',(0.,-0.75,1.5));
#12207=CARTESIAN_POINT('Origin',(0.,0.75,1.5));
#12208=CARTESIAN_POINT('',(0.,0.75,1.5));
#12209=CARTESIAN_POINT('',(0.,0.75,1.5));
#12210=CARTESIAN_POINT('',(22.,0.75,1.5));
#12211=CARTESIAN_POINT('',(22.,0.75,1.5));
#12212=CARTESIAN_POINT('',(0.,0.75,1.5));
#12213=CARTESIAN_POINT('Origin',(0.,0.75,1.3));
#12214=CARTESIAN_POINT('',(0.,0.75,1.3));
#12215=CARTESIAN_POINT('',(0.,0.75,1.3));
#12216=CARTESIAN_POINT('',(22.,0.75,1.3));
#12217=CARTESIAN_POINT('',(22.,0.75,1.3));
#12218=CARTESIAN_POINT('',(0.,0.75,1.3));
#12219=CARTESIAN_POINT('Origin',(0.,0.53,1.15));
#12220=CARTESIAN_POINT('',(0.,0.53,1.15));
#12221=CARTESIAN_POINT('',(0.,0.53,1.15));
#12222=CARTESIAN_POINT('',(22.,0.53,1.15));
#12223=CARTESIAN_POINT('',(22.,0.53,1.15));
#12224=CARTESIAN_POINT('',(0.,0.53,1.15));
#12225=CARTESIAN_POINT('Origin',(0.,0.53,1.));
#12226=CARTESIAN_POINT('',(0.,0.53,1.));
#12227=CARTESIAN_POINT('',(0.,0.53,1.));
#12228=CARTESIAN_POINT('',(22.,0.53,1.));
#12229=CARTESIAN_POINT('',(22.,0.53,1.));
#12230=CARTESIAN_POINT('',(0.,0.53,1.));
#12231=CARTESIAN_POINT('Origin',(0.,0.75,0.85));
#12232=CARTESIAN_POINT('',(0.,0.75,0.85));
#12233=CARTESIAN_POINT('',(0.,0.75,0.85));
#12234=CARTESIAN_POINT('',(22.,0.75,0.85));
#12235=CARTESIAN_POINT('',(22.,0.75,0.85));
#12236=CARTESIAN_POINT('',(0.,0.75,0.85));
#12237=CARTESIAN_POINT('Origin',(0.,0.75,0.));
#12238=CARTESIAN_POINT('',(0.,0.75,0.));
#12239=CARTESIAN_POINT('',(0.,0.75,0.));
#12240=CARTESIAN_POINT('',(22.,0.75,0.));
#12241=CARTESIAN_POINT('',(22.,0.75,0.));
#12242=CARTESIAN_POINT('',(0.,0.75,0.));
#12243=CARTESIAN_POINT('Origin',(0.,-0.75,0.));
#12244=CARTESIAN_POINT('',(0.,-0.75,0.));
#12245=CARTESIAN_POINT('',(0.,-0.75,0.));
#12246=CARTESIAN_POINT('',(22.,-0.75,0.));
#12247=CARTESIAN_POINT('',(22.,-0.75,0.));
#12248=CARTESIAN_POINT('',(0.,-0.75,0.));
#12249=CARTESIAN_POINT('Origin',(0.,-0.75,0.85));
#12250=CARTESIAN_POINT('',(0.,-0.75,0.85));
#12251=CARTESIAN_POINT('',(22.,-0.75,0.85));
#12252=CARTESIAN_POINT('Origin',(22.,0.,0.75));
#12253=CARTESIAN_POINT('Origin',(0.,0.,0.75));
#12254=CARTESIAN_POINT('',(0.,0.,0.));
#12255=CARTESIAN_POINT('Origin',(0.,0.395,0.25));
#12256=CARTESIAN_POINT('',(-0.5,0.3,0.25));
#12257=CARTESIAN_POINT('',(0.5,0.3,0.25));
#12258=CARTESIAN_POINT('',(0.25,0.3,0.25));
#12259=CARTESIAN_POINT('',(-0.5,0.5,0.25));
#12260=CARTESIAN_POINT('',(-0.5,0.5,0.25));
#12261=CARTESIAN_POINT('',(0.5,0.5,0.25));
#12262=CARTESIAN_POINT('',(0.5,0.5,0.25));
#12263=CARTESIAN_POINT('',(0.5,0.29,0.25));
#12264=CARTESIAN_POINT('Origin',(0.5,0.5,0.25));
#12265=CARTESIAN_POINT('',(-0.5,0.5,0.4));
#12266=CARTESIAN_POINT('',(-0.5,0.5,0.25));
#12267=CARTESIAN_POINT('',(0.5,0.5,0.4));
#12268=CARTESIAN_POINT('',(0.5,0.5,0.4));
#12269=CARTESIAN_POINT('',(0.5,0.5,0.25));
#12270=CARTESIAN_POINT('Origin',(0.,0.,0.4));
#12271=CARTESIAN_POINT('',(-0.5,-0.5,0.4));
#12272=CARTESIAN_POINT('',(-0.5,0.5,0.4));
#12273=CARTESIAN_POINT('',(0.5,-0.5,0.4));
#12274=CARTESIAN_POINT('',(-0.5,-0.5,0.4));
#12275=CARTESIAN_POINT('',(0.5,-0.3,0.4));
#12276=CARTESIAN_POINT('',(-0.2117,2.59257727379495E-17,0.4));
#12277=CARTESIAN_POINT('Origin',(0.,0.,0.4));
#12278=CARTESIAN_POINT('Origin',(-0.5,0.3,0.));
#12279=CARTESIAN_POINT('',(-0.5,0.3,0.15));
#12280=CARTESIAN_POINT('',(-0.5,0.3,0.));
#12281=CARTESIAN_POINT('',(-0.5,0.15,0.));
#12282=CARTESIAN_POINT('',(-0.5,0.225,0.075));
#12283=CARTESIAN_POINT('',(-0.5,-0.15,0.));
#12284=CARTESIAN_POINT('',(-0.5,0.3,0.));
#12285=CARTESIAN_POINT('',(-0.5,-0.3,0.15));
#12286=CARTESIAN_POINT('',(-0.5,-0.075,-0.075));
#12287=CARTESIAN_POINT('',(-0.5,-0.3,0.25));
#12288=CARTESIAN_POINT('',(-0.5,-0.3,0.));
#12289=CARTESIAN_POINT('',(-0.5,-0.5,0.25));
#12290=CARTESIAN_POINT('',(-0.5,-0.29,0.25));
#12291=CARTESIAN_POINT('',(-0.5,-0.5,0.25));
#12292=CARTESIAN_POINT('Origin',(-0.5,-0.5,0.25));
#12293=CARTESIAN_POINT('',(0.5,-0.5,0.25));
#12294=CARTESIAN_POINT('',(-0.5,-0.5,0.25));
#12295=CARTESIAN_POINT('',(0.5,-0.5,0.25));
#12296=CARTESIAN_POINT('Origin',(0.,-0.395,0.25));
#12297=CARTESIAN_POINT('',(0.5,-0.3,0.25));
#12298=CARTESIAN_POINT('',(-0.25,-0.3,0.25));
#12299=CARTESIAN_POINT('',(0.5,-0.5,0.25));
#12300=CARTESIAN_POINT('Origin',(0.5,-0.3,0.));
#12301=CARTESIAN_POINT('',(0.5,-0.3,0.15));
#12302=CARTESIAN_POINT('',(0.5,-0.3,0.));
#12303=CARTESIAN_POINT('',(0.5,-0.15,0.));
#12304=CARTESIAN_POINT('',(0.5,-0.225,0.075));
#12305=CARTESIAN_POINT('',(0.5,0.15,0.));
#12306=CARTESIAN_POINT('',(0.5,-0.3,0.));
#12307=CARTESIAN_POINT('',(0.5,0.3,0.15));
#12308=CARTESIAN_POINT('',(0.5,0.075,-0.075));
#12309=CARTESIAN_POINT('',(0.5,0.3,0.));
#12310=CARTESIAN_POINT('Origin',(-0.5,-0.3,0.));
#12311=CARTESIAN_POINT('',(-0.25,-0.3,0.15));
#12312=CARTESIAN_POINT('Origin',(-0.25,-0.225,0.075));
#12313=CARTESIAN_POINT('',(-0.149388386429468,-0.15,0.));
#12314=CARTESIAN_POINT('',(-0.25,-0.15,0.));
#12315=CARTESIAN_POINT('',(0.149388386429468,-0.15,0.));
#12316=CARTESIAN_POINT('Origin',(0.,0.,-0.15));
#12317=CARTESIAN_POINT('',(-0.25,-0.15,0.));
#12318=CARTESIAN_POINT('Origin',(0.,0.,-0.1));
#12319=CARTESIAN_POINT('',(-0.2117,-2.59257727379495E-17,0.));
#12320=CARTESIAN_POINT('Origin',(0.,0.,0.));
#12321=CARTESIAN_POINT('',(-0.2117,-2.59257727379495E-17,-0.1));
#12322=CARTESIAN_POINT('',(-0.149388386429468,0.15,0.));
#12323=CARTESIAN_POINT('Origin',(0.,0.,0.));
#12324=CARTESIAN_POINT('',(0.149388386429468,0.15,0.));
#12325=CARTESIAN_POINT('Origin',(0.,0.,-0.15));
#12326=CARTESIAN_POINT('Origin',(0.,0.,0.));
#12327=CARTESIAN_POINT('Origin',(0.,0.,0.));
#12328=CARTESIAN_POINT('',(0.25,0.15,0.));
#12329=CARTESIAN_POINT('Origin',(0.,0.,0.));
#12330=CARTESIAN_POINT('',(0.25,0.15,0.));
#12331=CARTESIAN_POINT('Origin',(0.25,0.225,0.075));
#12332=CARTESIAN_POINT('',(0.25,0.3,0.15));
#12333=CARTESIAN_POINT('Origin',(0.5,0.3,0.));
#12334=CARTESIAN_POINT('',(0.,0.,0.));
#12335=CARTESIAN_POINT('Origin',(0.,0.09,0.));
#12336=CARTESIAN_POINT('',(-0.285,0.1,3.49024337756996E-17));
#12337=CARTESIAN_POINT('Origin',(0.,0.1,0.));
#12338=CARTESIAN_POINT('',(-0.265,0.08,-3.24531401774049E-17));
#12339=CARTESIAN_POINT('',(-0.275,0.09,3.36777869765522E-17));
#12340=CARTESIAN_POINT('Origin',(0.,0.08,0.));
#12341=CARTESIAN_POINT('Origin',(0.,0.,0.));
#12342=CARTESIAN_POINT('',(-0.265,0.,3.24531401774049E-17));
#12343=CARTESIAN_POINT('',(-0.265,0.,3.24531401774049E-17));
#12344=CARTESIAN_POINT('Origin',(0.,0.,0.));
#12345=CARTESIAN_POINT('Origin',(0.,0.1,0.));
#12346=CARTESIAN_POINT('',(-0.5,0.1,6.12323399573677E-17));
#12347=CARTESIAN_POINT('Origin',(0.,0.1,0.));
#12348=CARTESIAN_POINT('Origin',(0.,0.,0.));
#12349=CARTESIAN_POINT('',(-0.5,0.,6.12323399573677E-17));
#12350=CARTESIAN_POINT('',(-0.5,0.,6.12323399573677E-17));
#12351=CARTESIAN_POINT('Origin',(0.,0.,0.));
#12352=CARTESIAN_POINT('Origin',(0.,0.,0.));
#12353=CARTESIAN_POINT('',(0.,0.,0.));
#12354=CARTESIAN_POINT('Origin',(0.115470053837925,-0.5,-0.2));
#12355=CARTESIAN_POINT('',(0.23094010767585,-0.5,0.));
#12356=CARTESIAN_POINT('',(0.115470053837925,-0.5,-0.2));
#12357=CARTESIAN_POINT('',(0.23094010767585,-0.5,0.));
#12358=CARTESIAN_POINT('',(0.115470053837925,-0.8,-0.2));
#12359=CARTESIAN_POINT('',(0.115470053837925,-0.5,-0.2));
#12360=CARTESIAN_POINT('',(0.23094010767585,-0.8,0.));
#12361=CARTESIAN_POINT('',(0.23094010767585,-0.8,0.));
#12362=CARTESIAN_POINT('',(0.23094010767585,-0.5,0.));
#12363=CARTESIAN_POINT('Origin',(-0.115470053837925,-0.5,-0.2));
#12364=CARTESIAN_POINT('',(-0.115470053837925,-0.5,-0.2));
#12365=CARTESIAN_POINT('',(0.115470053837925,-0.5,-0.2));
#12366=CARTESIAN_POINT('',(-0.115470053837925,-0.8,-0.2));
#12367=CARTESIAN_POINT('',(-0.115470053837925,-0.5,-0.2));
#12368=CARTESIAN_POINT('',(0.115470053837925,-0.8,-0.2));
#12369=CARTESIAN_POINT('Origin',(-0.23094010767585,-0.5,-2.77555756156289E-17));
#12370=CARTESIAN_POINT('',(-0.23094010767585,-0.5,-2.82820063659975E-17));
#12371=CARTESIAN_POINT('',(-0.115470053837925,-0.5,-0.2));
#12372=CARTESIAN_POINT('',(-0.23094010767585,-0.8,-2.77555756156289E-17));
#12373=CARTESIAN_POINT('',(-0.23094010767585,-0.5,-2.82820063659975E-17));
#12374=CARTESIAN_POINT('',(-0.115470053837925,-0.8,-0.2));
#12375=CARTESIAN_POINT('Origin',(-0.115470053837925,-0.5,0.2));
#12376=CARTESIAN_POINT('',(-0.115470053837925,-0.5,0.2));
#12377=CARTESIAN_POINT('',(-0.23094010767585,-0.5,-2.82820063659975E-17));
#12378=CARTESIAN_POINT('',(-0.115470053837925,-0.8,0.2));
#12379=CARTESIAN_POINT('',(-0.115470053837925,-0.5,0.2));
#12380=CARTESIAN_POINT('',(-0.23094010767585,-0.8,-2.82820063659975E-17));
#12381=CARTESIAN_POINT('Origin',(0.115470053837925,-0.5,0.2));
#12382=CARTESIAN_POINT('',(0.115470053837925,-0.5,0.2));
#12383=CARTESIAN_POINT('',(-0.115470053837925,-0.5,0.2));
#12384=CARTESIAN_POINT('',(0.115470053837925,-0.8,0.2));
#12385=CARTESIAN_POINT('',(0.115470053837925,-0.5,0.2));
#12386=CARTESIAN_POINT('',(-0.115470053837925,-0.8,0.2));
#12387=CARTESIAN_POINT('Origin',(0.23094010767585,-0.5,0.));
#12388=CARTESIAN_POINT('',(0.115470053837925,-0.5,0.2));
#12389=CARTESIAN_POINT('',(0.115470053837925,-0.8,0.2));
#12390=CARTESIAN_POINT('Origin',(0.,-0.5,0.));
#12391=CARTESIAN_POINT('Origin',(0.,-0.8,0.));
#12392=CARTESIAN_POINT('Origin',(0.,-1.9,0.));
#12393=CARTESIAN_POINT('',(-0.25,-1.9,3.06161699786838E-17));
#12394=CARTESIAN_POINT('Origin',(0.,-1.9,0.));
#12395=CARTESIAN_POINT('',(-0.24505,-1.9,3.00099698131059E-17));
#12396=CARTESIAN_POINT('Origin',(0.,-1.9,0.));
#12397=CARTESIAN_POINT('Origin',(0.,-3.,0.));
#12398=CARTESIAN_POINT('',(-0.25,-3.,3.06161699786838E-17));
#12399=CARTESIAN_POINT('',(-0.25,-3.,3.06161699786838E-17));
#12400=CARTESIAN_POINT('Origin',(0.,-3.,0.));
#12401=CARTESIAN_POINT('Origin',(0.,-3.,0.));
#12402=CARTESIAN_POINT('Origin',(0.375,0.5,0.));
#12403=CARTESIAN_POINT('',(-0.375,0.5,-4.59242549680257E-17));
#12404=CARTESIAN_POINT('Origin',(0.,0.5,0.));
#12405=CARTESIAN_POINT('Origin',(0.,0.475,0.));
#12406=CARTESIAN_POINT('',(-0.425,0.45,-5.20474889637625E-17));
#12407=CARTESIAN_POINT('Origin',(0.,0.45,0.));
#12408=CARTESIAN_POINT('',(-0.4,0.475,-4.89858719658941E-17));
#12409=CARTESIAN_POINT('Origin',(0.,0.24,0.));
#12410=CARTESIAN_POINT('',(-0.425,0.0299999999999998,-5.20474889637625E-17));
#12411=CARTESIAN_POINT('Origin',(0.,0.0299999999999998,0.));
#12412=CARTESIAN_POINT('',(-0.425,0.24,-5.20474889637625E-17));
#12413=CARTESIAN_POINT('Origin',(0.,0.0150000000000001,0.));
#12414=CARTESIAN_POINT('',(-0.395,4.85722573273506E-17,-4.83735485663204E-17));
#12415=CARTESIAN_POINT('Origin',(0.,0.,0.));
#12416=CARTESIAN_POINT('',(-0.41,0.0150000000000001,-5.02105187650415E-17));
#12417=CARTESIAN_POINT('Origin',(0.27,0.,0.));
#12418=CARTESIAN_POINT('',(-0.27,0.,-3.30654635769785E-17));
#12419=CARTESIAN_POINT('Origin',(0.,0.,0.));
#12420=CARTESIAN_POINT('Origin',(0.,-0.02,0.));
#12421=CARTESIAN_POINT('',(-0.24505,-0.0498999999999999,3.00099698131059E-17));
#12422=CARTESIAN_POINT('Origin',(0.,-0.0498999999999999,0.));
#12423=CARTESIAN_POINT('',(-0.26,-0.02,-3.18408167778312E-17));
#12424=CARTESIAN_POINT('Origin',(0.,-0.995,0.));
#12425=CARTESIAN_POINT('',(-0.24505,-0.995,-3.00099698131059E-17));
#12426=CARTESIAN_POINT('',(0.,0.,0.));
#12427=CARTESIAN_POINT('',(0.,0.,0.));
#12428=CARTESIAN_POINT('Origin',(-1.7,-2.5,15.));
#12429=CARTESIAN_POINT('',(-1.6,-2.5,15.225));
#12430=CARTESIAN_POINT('Origin',(-1.6,-2.5,15.));
#12431=CARTESIAN_POINT('',(-1.2,-2.5,15.225));
#12432=CARTESIAN_POINT('',(-1.7,-2.5,15.225));
#12433=CARTESIAN_POINT('Origin',(-1.2,-2.5,15.));
#12434=CARTESIAN_POINT('Origin',(-1.7,2.5,15.));
#12435=CARTESIAN_POINT('',(-1.6,2.5,15.225));
#12436=CARTESIAN_POINT('Origin',(-1.6,2.5,15.));
#12437=CARTESIAN_POINT('',(-1.2,2.5,15.225));
#12438=CARTESIAN_POINT('',(-1.7,2.5,15.225));
#12439=CARTESIAN_POINT('Origin',(-1.2,2.5,15.));
#12440=CARTESIAN_POINT('Origin',(-1.7,12.9,9.5));
#12441=CARTESIAN_POINT('',(-1.6,12.9,9.775));
#12442=CARTESIAN_POINT('Origin',(-1.6,12.9,9.5));
#12443=CARTESIAN_POINT('',(-1.2,12.9,9.775));
#12444=CARTESIAN_POINT('',(-1.7,12.9,9.775));
#12445=CARTESIAN_POINT('Origin',(-1.2,12.9,9.5));
#12446=CARTESIAN_POINT('Origin',(-1.7,9.1,12.5));
#12447=CARTESIAN_POINT('',(-1.6,9.1,12.775));
#12448=CARTESIAN_POINT('Origin',(-1.6,9.1,12.5));
#12449=CARTESIAN_POINT('',(-1.2,9.1,12.775));
#12450=CARTESIAN_POINT('',(-1.7,9.1,12.775));
#12451=CARTESIAN_POINT('Origin',(-1.2,9.1,12.5));
#12452=CARTESIAN_POINT('Origin',(-1.7,9.1,9.5));
#12453=CARTESIAN_POINT('',(-1.6,9.1,9.775));
#12454=CARTESIAN_POINT('Origin',(-1.6,9.1,9.5));
#12455=CARTESIAN_POINT('',(-1.2,9.1,9.775));
#12456=CARTESIAN_POINT('',(-1.7,9.1,9.775));
#12457=CARTESIAN_POINT('Origin',(-1.2,9.1,9.5));
#12458=CARTESIAN_POINT('Origin',(-1.7,12.9,12.5));
#12459=CARTESIAN_POINT('',(-1.6,12.9,12.775));
#12460=CARTESIAN_POINT('Origin',(-1.6,12.9,12.5));
#12461=CARTESIAN_POINT('',(-1.2,12.9,12.775));
#12462=CARTESIAN_POINT('',(-1.7,12.9,12.775));
#12463=CARTESIAN_POINT('Origin',(-1.2,12.9,12.5));
#12464=CARTESIAN_POINT('Origin',(-1.6,14.,14.5));
#12465=CARTESIAN_POINT('',(-1.2,8.,14.5));
#12466=CARTESIAN_POINT('',(-1.6,8.,14.5));
#12467=CARTESIAN_POINT('',(-1.6,8.,14.5));
#12468=CARTESIAN_POINT('',(-1.2,14.,14.5));
#12469=CARTESIAN_POINT('',(-1.2,14.,14.5));
#12470=CARTESIAN_POINT('',(-1.6,14.,14.5));
#12471=CARTESIAN_POINT('',(-1.6,14.,14.5));
#12472=CARTESIAN_POINT('',(-1.6,14.,14.5));
#12473=CARTESIAN_POINT('Origin',(-1.6,7.,7.5));
#12474=CARTESIAN_POINT('',(-1.6,8.,7.5));
#12475=CARTESIAN_POINT('',(-1.2,8.,7.5));
#12476=CARTESIAN_POINT('',(-1.6,8.,7.5));
#12477=CARTESIAN_POINT('',(-1.6,14.,7.5));
#12478=CARTESIAN_POINT('',(-1.6,7.,7.5));
#12479=CARTESIAN_POINT('',(-1.2,14.,7.5));
#12480=CARTESIAN_POINT('',(-1.6,14.,7.5));
#12481=CARTESIAN_POINT('',(-1.2,7.,7.5));
#12482=CARTESIAN_POINT('Origin',(-1.6,14.,7.5));
#12483=CARTESIAN_POINT('',(-1.6,14.,7.5));
#12484=CARTESIAN_POINT('',(-1.2,14.,7.5));
#12485=CARTESIAN_POINT('Origin',(-1.6,0.,10.));
#12486=CARTESIAN_POINT('',(-1.6,8.,3.5));
#12487=CARTESIAN_POINT('',(-1.6,8.,3.5));
#12488=CARTESIAN_POINT('',(-1.6,-8.,3.5));
#12489=CARTESIAN_POINT('',(-1.6,-8.,3.5));
#12490=CARTESIAN_POINT('',(-1.6,-8.,16.5));
#12491=CARTESIAN_POINT('',(-1.6,-8.,16.5));
#12492=CARTESIAN_POINT('',(-1.6,8.,16.5));
#12493=CARTESIAN_POINT('',(-1.6,8.,16.5));
#12494=CARTESIAN_POINT('',(-1.6,8.,3.5));
#12495=CARTESIAN_POINT('Origin',(-1.6,8.,3.5));
#12496=CARTESIAN_POINT('',(-1.2,8.,3.5));
#12497=CARTESIAN_POINT('',(-1.2,8.,3.5));
#12498=CARTESIAN_POINT('',(-1.6,8.,3.5));
#12499=CARTESIAN_POINT('Origin',(-1.6,8.,16.5));
#12500=CARTESIAN_POINT('',(-1.2,-8.,16.5));
#12501=CARTESIAN_POINT('',(-1.6,-8.,16.5));
#12502=CARTESIAN_POINT('',(-1.2,8.,16.5));
#12503=CARTESIAN_POINT('',(-1.2,8.,16.5));
#12504=CARTESIAN_POINT('',(-1.6,8.,16.5));
#12505=CARTESIAN_POINT('Origin',(-1.6,8.,3.5));
#12506=CARTESIAN_POINT('',(-1.2,8.,3.5));
#12507=CARTESIAN_POINT('Origin',(-1.6,-8.,3.5));
#12508=CARTESIAN_POINT('',(-1.2,-8.,3.5));
#12509=CARTESIAN_POINT('',(-1.2,-8.,3.5));
#12510=CARTESIAN_POINT('',(-1.6,-8.,3.5));
#12511=CARTESIAN_POINT('Origin',(-1.6,-8.,16.5));
#12512=CARTESIAN_POINT('',(-1.2,-8.,16.5));
#12513=CARTESIAN_POINT('Origin',(-1.2,0.,10.));
#12514=CARTESIAN_POINT('',(0.,0.,0.));
#12515=CARTESIAN_POINT('Origin',(-2.9,-2.5,15.));
#12516=CARTESIAN_POINT('',(-2.9,-2.5,15.165));
#12517=CARTESIAN_POINT('Origin',(-2.9,-2.5,15.));
#12518=CARTESIAN_POINT('',(-1.6,-2.5,15.165));
#12519=CARTESIAN_POINT('',(-2.9,-2.5,15.165));
#12520=CARTESIAN_POINT('Origin',(-1.6,-2.5,15.));
#12521=CARTESIAN_POINT('Origin',(-2.9,-2.5,15.));
#12522=CARTESIAN_POINT('Origin',(-2.9,2.5,15.));
#12523=CARTESIAN_POINT('',(-2.9,2.5,15.165));
#12524=CARTESIAN_POINT('Origin',(-2.9,2.5,15.));
#12525=CARTESIAN_POINT('',(-1.6,2.5,15.165));
#12526=CARTESIAN_POINT('',(-2.9,2.5,15.165));
#12527=CARTESIAN_POINT('Origin',(-1.6,2.5,15.));
#12528=CARTESIAN_POINT('Origin',(-2.9,2.5,15.));
#12529=CARTESIAN_POINT('Origin',(-3.,2.5,15.));
#12530=CARTESIAN_POINT('',(-1.6,2.5,15.5));
#12531=CARTESIAN_POINT('Origin',(-1.6,2.5,15.));
#12532=CARTESIAN_POINT('',(-3.,2.5,15.5));
#12533=CARTESIAN_POINT('',(-3.,2.5,15.5));
#12534=CARTESIAN_POINT('',(-3.,2.5,14.5));
#12535=CARTESIAN_POINT('Origin',(-3.,2.5,15.));
#12536=CARTESIAN_POINT('Origin',(-3.,2.5,15.));
#12537=CARTESIAN_POINT('Origin',(-1.6,2.5,15.));
#12538=CARTESIAN_POINT('Origin',(-3.,2.5,15.));
#12539=CARTESIAN_POINT('',(-3.,2.5,15.));
#12540=CARTESIAN_POINT('Origin',(-3.,2.5,15.));
#12541=CARTESIAN_POINT('',(-3.5,2.5,15.));
#12542=CARTESIAN_POINT('Origin',(-3.,2.5,15.));
#12543=CARTESIAN_POINT('Origin',(-3.,2.5,15.));
#12544=CARTESIAN_POINT('Origin',(-3.,-2.5,15.));
#12545=CARTESIAN_POINT('',(-1.6,-2.5,15.5));
#12546=CARTESIAN_POINT('Origin',(-1.6,-2.5,15.));
#12547=CARTESIAN_POINT('',(-3.,-2.5,15.5));
#12548=CARTESIAN_POINT('',(-3.,-2.5,15.5));
#12549=CARTESIAN_POINT('',(-3.,-2.5,14.5));
#12550=CARTESIAN_POINT('Origin',(-3.,-2.5,15.));
#12551=CARTESIAN_POINT('Origin',(-3.,-2.5,15.));
#12552=CARTESIAN_POINT('Origin',(-1.6,-2.5,15.));
#12553=CARTESIAN_POINT('Origin',(-3.,-2.5,15.));
#12554=CARTESIAN_POINT('',(-3.,-2.5,15.));
#12555=CARTESIAN_POINT('Origin',(-3.,-2.5,15.));
#12556=CARTESIAN_POINT('',(-3.5,-2.5,15.));
#12557=CARTESIAN_POINT('Origin',(-3.,-2.5,15.));
#12558=CARTESIAN_POINT('Origin',(-3.,-2.5,15.));
#12559=CARTESIAN_POINT('Origin',(-3.,-2.5,15.));
#12560=CARTESIAN_POINT('',(-3.5,-2.5,15.));
#12561=CARTESIAN_POINT('',(0.,0.,0.));
#12562=CARTESIAN_POINT('',(0.,0.,0.));
#12563=CARTESIAN_POINT('Origin',(1.5,-1.9,1.7));
#12564=CARTESIAN_POINT('',(1.56403124237433,-1.7,1.7));
#12565=CARTESIAN_POINT('',(1.43596875762567,-1.7,1.7));
#12566=CARTESIAN_POINT('',(0.75,-1.7,1.7));
#12567=CARTESIAN_POINT('Origin',(1.5,-1.9,1.7));
#12568=CARTESIAN_POINT('Origin',(1.5,-1.9,1.7));
#12569=CARTESIAN_POINT('',(1.56403124237433,-1.7,1.75));
#12570=CARTESIAN_POINT('',(1.56403124237433,-1.7,1.7));
#12571=CARTESIAN_POINT('',(1.29,-1.9,1.75));
#12572=CARTESIAN_POINT('Origin',(1.5,-1.9,1.75));
#12573=CARTESIAN_POINT('',(1.29,-1.9,2.4));
#12574=CARTESIAN_POINT('',(1.29,-1.9,1.7));
#12575=CARTESIAN_POINT('Origin',(1.5,-1.9,2.4));
#12576=CARTESIAN_POINT('',(1.43596875762567,-1.7,1.75));
#12577=CARTESIAN_POINT('Origin',(1.5,-1.9,1.75));
#12578=CARTESIAN_POINT('',(1.43596875762567,-1.7,1.7));
#12579=CARTESIAN_POINT('Origin',(-1.5,1.9,1.7));
#12580=CARTESIAN_POINT('',(-1.56403124237433,1.7,1.7));
#12581=CARTESIAN_POINT('',(-1.43596875762567,1.7,1.7));
#12582=CARTESIAN_POINT('',(-0.75,1.7,1.7));
#12583=CARTESIAN_POINT('Origin',(-1.5,1.9,1.7));
#12584=CARTESIAN_POINT('Origin',(-1.5,1.9,1.7));
#12585=CARTESIAN_POINT('',(-1.56403124237433,1.7,1.75));
#12586=CARTESIAN_POINT('',(-1.56403124237433,1.7,1.7));
#12587=CARTESIAN_POINT('',(-1.71,1.9,1.75));
#12588=CARTESIAN_POINT('Origin',(-1.5,1.9,1.75));
#12589=CARTESIAN_POINT('',(-1.71,1.9,2.4));
#12590=CARTESIAN_POINT('',(-1.71,1.9,1.7));
#12591=CARTESIAN_POINT('Origin',(-1.5,1.9,2.4));
#12592=CARTESIAN_POINT('',(-1.43596875762567,1.7,1.75));
#12593=CARTESIAN_POINT('Origin',(-1.5,1.9,1.75));
#12594=CARTESIAN_POINT('',(-1.43596875762567,1.7,1.7));
#12595=CARTESIAN_POINT('Origin',(-1.5,-1.9,1.7));
#12596=CARTESIAN_POINT('',(-1.43596875762567,-1.7,1.7));
#12597=CARTESIAN_POINT('',(-1.56403124237433,-1.7,1.7));
#12598=CARTESIAN_POINT('',(-0.75,-1.7,1.7));
#12599=CARTESIAN_POINT('Origin',(-1.5,-1.9,1.7));
#12600=CARTESIAN_POINT('Origin',(-1.5,-1.9,1.7));
#12601=CARTESIAN_POINT('',(-1.43596875762567,-1.7,1.75));
#12602=CARTESIAN_POINT('',(-1.43596875762567,-1.7,1.7));
#12603=CARTESIAN_POINT('',(-1.71,-1.9,1.75));
#12604=CARTESIAN_POINT('Origin',(-1.5,-1.9,1.75));
#12605=CARTESIAN_POINT('',(-1.71,-1.9,2.4));
#12606=CARTESIAN_POINT('',(-1.71,-1.9,1.7));
#12607=CARTESIAN_POINT('Origin',(-1.5,-1.9,2.4));
#12608=CARTESIAN_POINT('',(-1.56403124237433,-1.7,1.75));
#12609=CARTESIAN_POINT('Origin',(-1.5,-1.9,1.75));
#12610=CARTESIAN_POINT('',(-1.56403124237433,-1.7,1.7));
#12611=CARTESIAN_POINT('Origin',(1.5,1.9,1.7));
#12612=CARTESIAN_POINT('',(1.43596875762567,1.7,1.7));
#12613=CARTESIAN_POINT('',(1.56403124237433,1.7,1.7));
#12614=CARTESIAN_POINT('',(0.75,1.7,1.7));
#12615=CARTESIAN_POINT('Origin',(1.5,1.9,1.7));
#12616=CARTESIAN_POINT('Origin',(1.5,1.9,1.7));
#12617=CARTESIAN_POINT('',(1.43596875762567,1.7,1.75));
#12618=CARTESIAN_POINT('',(1.43596875762567,1.7,1.7));
#12619=CARTESIAN_POINT('',(1.29,1.9,1.75));
#12620=CARTESIAN_POINT('Origin',(1.5,1.9,1.75));
#12621=CARTESIAN_POINT('',(1.29,1.9,2.4));
#12622=CARTESIAN_POINT('',(1.29,1.9,1.7));
#12623=CARTESIAN_POINT('Origin',(1.5,1.9,2.4));
#12624=CARTESIAN_POINT('',(1.56403124237433,1.7,1.75));
#12625=CARTESIAN_POINT('Origin',(1.5,1.9,1.75));
#12626=CARTESIAN_POINT('',(1.56403124237433,1.7,1.7));
#12627=CARTESIAN_POINT('Origin',(0.,-1.7,1.75));
#12628=CARTESIAN_POINT('',(0.,-1.7,1.75));
#12629=CARTESIAN_POINT('',(-1.97,-1.7,1.75));
#12630=CARTESIAN_POINT('',(0.,-1.7,1.75));
#12631=CARTESIAN_POINT('',(-1.97,-1.7,0.43));
#12632=CARTESIAN_POINT('',(-1.97,-1.7,1.75));
#12633=CARTESIAN_POINT('',(1.97,-1.7,0.43));
#12634=CARTESIAN_POINT('',(0.,-1.7,0.43));
#12635=CARTESIAN_POINT('',(1.97,-1.7,1.75));
#12636=CARTESIAN_POINT('',(1.97,-1.7,1.75));
#12637=CARTESIAN_POINT('',(0.,-1.7,1.75));
#12638=CARTESIAN_POINT('Origin',(0.,1.7,0.43));
#12639=CARTESIAN_POINT('',(0.,1.7,1.75));
#12640=CARTESIAN_POINT('',(1.97,1.7,1.75));
#12641=CARTESIAN_POINT('',(0.,1.7,1.75));
#12642=CARTESIAN_POINT('',(1.97,1.7,0.43));
#12643=CARTESIAN_POINT('',(1.97,1.7,0.43));
#12644=CARTESIAN_POINT('',(-1.97,1.7,0.43));
#12645=CARTESIAN_POINT('',(0.,1.7,0.43));
#12646=CARTESIAN_POINT('',(-1.97,1.7,1.75));
#12647=CARTESIAN_POINT('',(-1.97,1.7,0.43));
#12648=CARTESIAN_POINT('',(0.,1.7,1.75));
#12649=CARTESIAN_POINT('Origin',(-1.97,0.,1.415));
#12650=CARTESIAN_POINT('',(-1.97,-2.35,1.75));
#12651=CARTESIAN_POINT('',(-1.97,-2.35,1.75));
#12652=CARTESIAN_POINT('',(-1.97,-2.35,2.4));
#12653=CARTESIAN_POINT('',(-1.97,-2.35,2.4));
#12654=CARTESIAN_POINT('',(-1.97,2.35,2.4));
#12655=CARTESIAN_POINT('',(-1.97,2.35,2.4));
#12656=CARTESIAN_POINT('',(-1.97,2.35,1.75));
#12657=CARTESIAN_POINT('',(-1.97,2.35,1.75));
#12658=CARTESIAN_POINT('',(-1.97,1.7,1.75));
#12659=CARTESIAN_POINT('',(-1.97,0.78,0.43));
#12660=CARTESIAN_POINT('',(-1.97,0.78,0.43));
#12661=CARTESIAN_POINT('',(-1.97,0.78,1.55));
#12662=CARTESIAN_POINT('',(-1.97,0.78,1.55));
#12663=CARTESIAN_POINT('',(-1.97,-0.78,1.55));
#12664=CARTESIAN_POINT('',(-1.97,-0.78,1.55));
#12665=CARTESIAN_POINT('',(-1.97,-0.78,0.43));
#12666=CARTESIAN_POINT('',(-1.97,-0.78,0.43));
#12667=CARTESIAN_POINT('',(-1.97,-1.7,0.43));
#12668=CARTESIAN_POINT('Origin',(0.,-2.35,1.75));
#12669=CARTESIAN_POINT('',(1.97,-2.35,1.75));
#12670=CARTESIAN_POINT('',(1.97,-2.35,1.75));
#12671=CARTESIAN_POINT('',(0.,-2.35,1.75));
#12672=CARTESIAN_POINT('Origin',(0.,-2.35,2.4));
#12673=CARTESIAN_POINT('',(1.97,-2.35,2.4));
#12674=CARTESIAN_POINT('',(1.97,-2.35,2.4));
#12675=CARTESIAN_POINT('',(0.,-2.35,2.4));
#12676=CARTESIAN_POINT('Origin',(0.,2.35,2.4));
#12677=CARTESIAN_POINT('',(1.97,2.35,2.4));
#12678=CARTESIAN_POINT('',(1.97,2.35,2.4));
#12679=CARTESIAN_POINT('',(0.,2.35,2.4));
#12680=CARTESIAN_POINT('Origin',(0.,2.35,1.75));
#12681=CARTESIAN_POINT('',(1.97,2.35,1.75));
#12682=CARTESIAN_POINT('',(1.97,2.35,1.75));
#12683=CARTESIAN_POINT('',(0.,2.35,1.75));
#12684=CARTESIAN_POINT('Origin',(0.,1.7,1.75));
#12685=CARTESIAN_POINT('',(1.97,1.7,1.75));
#12686=CARTESIAN_POINT('Origin',(0.,0.78,0.43));
#12687=CARTESIAN_POINT('',(1.97,0.78,0.43));
#12688=CARTESIAN_POINT('',(1.97,0.78,0.43));
#12689=CARTESIAN_POINT('',(0.,0.78,0.43));
#12690=CARTESIAN_POINT('Origin',(0.,0.78,1.55));
#12691=CARTESIAN_POINT('',(1.97,0.78,1.55));
#12692=CARTESIAN_POINT('',(1.97,0.78,1.55));
#12693=CARTESIAN_POINT('',(0.,0.78,1.55));
#12694=CARTESIAN_POINT('Origin',(0.,-0.78,1.55));
#12695=CARTESIAN_POINT('',(1.97,-0.78,1.55));
#12696=CARTESIAN_POINT('',(1.97,-0.78,1.55));
#12697=CARTESIAN_POINT('',(0.,-0.78,1.55));
#12698=CARTESIAN_POINT('Origin',(0.,-0.78,0.43));
#12699=CARTESIAN_POINT('',(1.97,-0.78,0.43));
#12700=CARTESIAN_POINT('',(1.97,-0.78,0.43));
#12701=CARTESIAN_POINT('',(0.,-0.78,0.43));
#12702=CARTESIAN_POINT('Origin',(0.,-1.7,0.43));
#12703=CARTESIAN_POINT('',(1.97,-1.7,0.43));
#12704=CARTESIAN_POINT('Origin',(1.97,0.,1.415));
#12705=CARTESIAN_POINT('',(0.,0.,0.));
#12706=CARTESIAN_POINT('Origin',(1.97,1.7,2.3));
#12707=CARTESIAN_POINT('',(1.97,1.7,2.3));
#12708=CARTESIAN_POINT('',(1.97,-1.7,2.3));
#12709=CARTESIAN_POINT('',(1.97,1.7,2.3));
#12710=CARTESIAN_POINT('',(3.07,-1.7,2.3));
#12711=CARTESIAN_POINT('',(1.97,-1.7,2.3));
#12712=CARTESIAN_POINT('',(3.07,1.7,2.3));
#12713=CARTESIAN_POINT('',(3.07,1.7,2.3));
#12714=CARTESIAN_POINT('',(1.97,1.7,2.3));
#12715=CARTESIAN_POINT('Origin',(1.97,1.7,0.46));
#12716=CARTESIAN_POINT('',(1.97,1.7,0.46));
#12717=CARTESIAN_POINT('',(1.97,1.7,0.46));
#12718=CARTESIAN_POINT('',(3.07,1.7,0.46));
#12719=CARTESIAN_POINT('',(3.07,1.7,0.46));
#12720=CARTESIAN_POINT('',(1.97,1.7,0.46));
#12721=CARTESIAN_POINT('Origin',(1.97,0.78,0.46));
#12722=CARTESIAN_POINT('',(1.97,0.78,0.46));
#12723=CARTESIAN_POINT('',(1.97,0.78,0.46));
#12724=CARTESIAN_POINT('',(3.07,0.78,0.46));
#12725=CARTESIAN_POINT('',(3.07,0.78,0.46));
#12726=CARTESIAN_POINT('',(1.97,0.78,0.46));
#12727=CARTESIAN_POINT('Origin',(1.97,0.78,1.55));
#12728=CARTESIAN_POINT('',(1.97,0.78,1.55));
#12729=CARTESIAN_POINT('',(1.97,0.78,1.55));
#12730=CARTESIAN_POINT('',(3.07,0.78,1.55));
#12731=CARTESIAN_POINT('',(3.07,0.78,1.55));
#12732=CARTESIAN_POINT('',(1.97,0.78,1.55));
#12733=CARTESIAN_POINT('Origin',(1.97,-0.78,1.55));
#12734=CARTESIAN_POINT('',(1.97,-0.78,1.55));
#12735=CARTESIAN_POINT('',(1.97,-0.78,1.55));
#12736=CARTESIAN_POINT('',(3.07,-0.78,1.55));
#12737=CARTESIAN_POINT('',(3.07,-0.78,1.55));
#12738=CARTESIAN_POINT('',(1.97,-0.78,1.55));
#12739=CARTESIAN_POINT('Origin',(1.97,-0.78,0.46));
#12740=CARTESIAN_POINT('',(1.97,-0.78,0.46));
#12741=CARTESIAN_POINT('',(1.97,-0.78,0.46));
#12742=CARTESIAN_POINT('',(3.07,-0.78,0.46));
#12743=CARTESIAN_POINT('',(3.07,-0.78,0.46));
#12744=CARTESIAN_POINT('',(1.97,-0.78,0.46));
#12745=CARTESIAN_POINT('Origin',(1.97,-1.7,0.46));
#12746=CARTESIAN_POINT('',(1.97,-1.7,0.46));
#12747=CARTESIAN_POINT('',(1.97,-1.7,0.46));
#12748=CARTESIAN_POINT('',(3.07,-1.7,0.46));
#12749=CARTESIAN_POINT('',(3.07,-1.7,0.46));
#12750=CARTESIAN_POINT('',(1.97,-1.7,0.46));
#12751=CARTESIAN_POINT('Origin',(1.97,-1.7,2.3));
#12752=CARTESIAN_POINT('',(1.97,-1.7,2.3));
#12753=CARTESIAN_POINT('',(3.07,-1.7,2.3));
#12754=CARTESIAN_POINT('Origin',(3.07,0.,1.38));
#12755=CARTESIAN_POINT('Origin',(1.97,0.,1.38));
#12756=CARTESIAN_POINT('',(0.,0.,0.));
#12757=CARTESIAN_POINT('Origin',(-1.97,-0.78,0.46));
#12758=CARTESIAN_POINT('',(-1.97,-1.7,0.46));
#12759=CARTESIAN_POINT('',(-1.97,-0.78,0.46));
#12760=CARTESIAN_POINT('',(-1.97,-1.7,0.46));
#12761=CARTESIAN_POINT('',(-3.07,-1.7,0.46));
#12762=CARTESIAN_POINT('',(-1.97,-1.7,0.46));
#12763=CARTESIAN_POINT('',(-3.07,-0.78,0.46));
#12764=CARTESIAN_POINT('',(-3.07,-1.7,0.46));
#12765=CARTESIAN_POINT('',(-1.97,-0.78,0.46));
#12766=CARTESIAN_POINT('Origin',(-1.97,-0.78,1.55));
#12767=CARTESIAN_POINT('',(-1.97,-0.78,1.55));
#12768=CARTESIAN_POINT('',(-1.97,-0.78,0.46));
#12769=CARTESIAN_POINT('',(-3.07,-0.78,1.55));
#12770=CARTESIAN_POINT('',(-3.07,-0.78,0.46));
#12771=CARTESIAN_POINT('',(-1.97,-0.78,1.55));
#12772=CARTESIAN_POINT('Origin',(-1.97,0.78,1.55));
#12773=CARTESIAN_POINT('',(-1.97,0.78,1.55));
#12774=CARTESIAN_POINT('',(-1.97,-0.78,1.55));
#12775=CARTESIAN_POINT('',(-3.07,0.78,1.55));
#12776=CARTESIAN_POINT('',(-3.07,-0.78,1.55));
#12777=CARTESIAN_POINT('',(-1.97,0.78,1.55));
#12778=CARTESIAN_POINT('Origin',(-1.97,0.78,0.46));
#12779=CARTESIAN_POINT('',(-1.97,0.78,0.46));
#12780=CARTESIAN_POINT('',(-1.97,0.78,1.55));
#12781=CARTESIAN_POINT('',(-3.07,0.78,0.46));
#12782=CARTESIAN_POINT('',(-3.07,0.78,1.55));
#12783=CARTESIAN_POINT('',(-1.97,0.78,0.46));
#12784=CARTESIAN_POINT('Origin',(-1.97,1.7,0.46));
#12785=CARTESIAN_POINT('',(-1.97,1.7,0.46));
#12786=CARTESIAN_POINT('',(-1.97,0.78,0.46));
#12787=CARTESIAN_POINT('',(-3.07,1.7,0.46));
#12788=CARTESIAN_POINT('',(-3.07,0.78,0.46));
#12789=CARTESIAN_POINT('',(-1.97,1.7,0.46));
#12790=CARTESIAN_POINT('Origin',(-1.97,1.7,2.3));
#12791=CARTESIAN_POINT('',(-1.97,1.7,2.3));
#12792=CARTESIAN_POINT('',(-1.97,1.7,0.46));
#12793=CARTESIAN_POINT('',(-3.07,1.7,2.3));
#12794=CARTESIAN_POINT('',(-3.07,1.7,0.46));
#12795=CARTESIAN_POINT('',(-1.97,1.7,2.3));
#12796=CARTESIAN_POINT('Origin',(-1.97,-1.7,2.3));
#12797=CARTESIAN_POINT('',(-1.97,-1.7,2.3));
#12798=CARTESIAN_POINT('',(-1.97,1.7,2.3));
#12799=CARTESIAN_POINT('',(-3.07,-1.7,2.3));
#12800=CARTESIAN_POINT('',(-3.07,1.7,2.3));
#12801=CARTESIAN_POINT('',(-1.97,-1.7,2.3));
#12802=CARTESIAN_POINT('Origin',(-1.97,-1.7,0.46));
#12803=CARTESIAN_POINT('',(-1.97,-1.7,2.3));
#12804=CARTESIAN_POINT('',(-3.07,-1.7,2.3));
#12805=CARTESIAN_POINT('Origin',(-1.97,0.,1.38));
#12806=CARTESIAN_POINT('Origin',(-3.07,0.,1.38));
#12807=CARTESIAN_POINT('',(0.,0.,0.));
#12808=CARTESIAN_POINT('',(0.,0.,0.));
#12809=CARTESIAN_POINT('',(0.,0.,0.));
#12810=CARTESIAN_POINT('',(0.,0.,0.));
#12811=CARTESIAN_POINT('Origin',(0.115470053837925,-0.5,-0.2));
#12812=CARTESIAN_POINT('',(0.23094010767585,-0.5,0.));
#12813=CARTESIAN_POINT('',(0.115470053837925,-0.5,-0.2));
#12814=CARTESIAN_POINT('',(0.23094010767585,-0.5,0.));
#12815=CARTESIAN_POINT('',(0.115470053837925,-0.8,-0.2));
#12816=CARTESIAN_POINT('',(0.115470053837925,-0.5,-0.2));
#12817=CARTESIAN_POINT('',(0.23094010767585,-0.8,0.));
#12818=CARTESIAN_POINT('',(0.23094010767585,-0.8,0.));
#12819=CARTESIAN_POINT('',(0.23094010767585,-0.5,0.));
#12820=CARTESIAN_POINT('Origin',(-0.115470053837925,-0.5,-0.2));
#12821=CARTESIAN_POINT('',(-0.115470053837925,-0.5,-0.2));
#12822=CARTESIAN_POINT('',(0.115470053837925,-0.5,-0.2));
#12823=CARTESIAN_POINT('',(-0.115470053837925,-0.8,-0.2));
#12824=CARTESIAN_POINT('',(-0.115470053837925,-0.5,-0.2));
#12825=CARTESIAN_POINT('',(0.115470053837925,-0.8,-0.2));
#12826=CARTESIAN_POINT('Origin',(-0.23094010767585,-0.5,-2.77555756156289E-17));
#12827=CARTESIAN_POINT('',(-0.23094010767585,-0.5,-2.82820063659975E-17));
#12828=CARTESIAN_POINT('',(-0.115470053837925,-0.5,-0.2));
#12829=CARTESIAN_POINT('',(-0.23094010767585,-0.8,-2.77555756156289E-17));
#12830=CARTESIAN_POINT('',(-0.23094010767585,-0.5,-2.82820063659975E-17));
#12831=CARTESIAN_POINT('',(-0.115470053837925,-0.8,-0.2));
#12832=CARTESIAN_POINT('Origin',(-0.115470053837925,-0.5,0.2));
#12833=CARTESIAN_POINT('',(-0.115470053837925,-0.5,0.2));
#12834=CARTESIAN_POINT('',(-0.23094010767585,-0.5,-2.82820063659975E-17));
#12835=CARTESIAN_POINT('',(-0.115470053837925,-0.8,0.2));
#12836=CARTESIAN_POINT('',(-0.115470053837925,-0.5,0.2));
#12837=CARTESIAN_POINT('',(-0.23094010767585,-0.8,-2.82820063659975E-17));
#12838=CARTESIAN_POINT('Origin',(0.115470053837925,-0.5,0.2));
#12839=CARTESIAN_POINT('',(0.115470053837925,-0.5,0.2));
#12840=CARTESIAN_POINT('',(-0.115470053837925,-0.5,0.2));
#12841=CARTESIAN_POINT('',(0.115470053837925,-0.8,0.2));
#12842=CARTESIAN_POINT('',(0.115470053837925,-0.5,0.2));
#12843=CARTESIAN_POINT('',(-0.115470053837925,-0.8,0.2));
#12844=CARTESIAN_POINT('Origin',(0.23094010767585,-0.5,0.));
#12845=CARTESIAN_POINT('',(0.115470053837925,-0.5,0.2));
#12846=CARTESIAN_POINT('',(0.115470053837925,-0.8,0.2));
#12847=CARTESIAN_POINT('Origin',(0.,-0.5,0.));
#12848=CARTESIAN_POINT('Origin',(0.,-0.8,0.));
#12849=CARTESIAN_POINT('Origin',(0.,-1.4,0.));
#12850=CARTESIAN_POINT('',(-0.24505,-1.4,3.00099698131059E-17));
#12851=CARTESIAN_POINT('Origin',(0.,-1.4,0.));
#12852=CARTESIAN_POINT('Origin',(0.375,0.5,0.));
#12853=CARTESIAN_POINT('',(-0.375,0.5,-4.59242549680257E-17));
#12854=CARTESIAN_POINT('Origin',(0.,0.5,0.));
#12855=CARTESIAN_POINT('Origin',(0.,0.475,0.));
#12856=CARTESIAN_POINT('',(-0.425,0.45,-5.20474889637625E-17));
#12857=CARTESIAN_POINT('Origin',(0.,0.45,0.));
#12858=CARTESIAN_POINT('',(-0.4,0.475,-4.89858719658941E-17));
#12859=CARTESIAN_POINT('Origin',(0.,0.24,0.));
#12860=CARTESIAN_POINT('',(-0.425,0.0299999999999998,-5.20474889637625E-17));
#12861=CARTESIAN_POINT('Origin',(0.,0.0299999999999998,0.));
#12862=CARTESIAN_POINT('',(-0.425,0.24,-5.20474889637625E-17));
#12863=CARTESIAN_POINT('Origin',(0.,0.0150000000000001,0.));
#12864=CARTESIAN_POINT('',(-0.395,4.85722573273506E-17,-4.83735485663204E-17));
#12865=CARTESIAN_POINT('Origin',(0.,0.,0.));
#12866=CARTESIAN_POINT('',(-0.41,0.0150000000000001,-5.02105187650415E-17));
#12867=CARTESIAN_POINT('Origin',(0.27,0.,0.));
#12868=CARTESIAN_POINT('',(-0.27,0.,-3.30654635769785E-17));
#12869=CARTESIAN_POINT('Origin',(0.,0.,0.));
#12870=CARTESIAN_POINT('Origin',(0.,-0.02,0.));
#12871=CARTESIAN_POINT('',(-0.24505,-0.0498999999999999,3.00099698131059E-17));
#12872=CARTESIAN_POINT('Origin',(0.,-0.0498999999999999,0.));
#12873=CARTESIAN_POINT('',(-0.26,-0.02,-3.18408167778312E-17));
#12874=CARTESIAN_POINT('Origin',(0.,-0.995,0.));
#12875=CARTESIAN_POINT('',(-0.24505,-0.995,-3.00099698131059E-17));
#12876=CARTESIAN_POINT('',(0.,0.,0.));
#12877=CARTESIAN_POINT('Origin',(0.3,0.4,0.));
#12878=CARTESIAN_POINT('',(-0.3,0.4,-3.67394039744206E-17));
#12879=CARTESIAN_POINT('Origin',(0.,0.4,0.));
#12880=CARTESIAN_POINT('Origin',(0.,0.375,0.));
#12881=CARTESIAN_POINT('',(-0.35,0.35,-4.28626379701573E-17));
#12882=CARTESIAN_POINT('Origin',(0.,0.35,0.));
#12883=CARTESIAN_POINT('',(-0.325,0.375,-3.9801020972289E-17));
#12884=CARTESIAN_POINT('Origin',(0.,0.19,0.));
#12885=CARTESIAN_POINT('',(-0.35,0.03,-4.28626379701574E-17));
#12886=CARTESIAN_POINT('Origin',(0.,0.03,0.));
#12887=CARTESIAN_POINT('',(-0.35,0.19,-4.28626379701574E-17));
#12888=CARTESIAN_POINT('Origin',(0.,0.0149999999999999,0.));
#12889=CARTESIAN_POINT('',(-0.32,-3.29597460435593E-17,-3.91886975727153E-17));
#12890=CARTESIAN_POINT('Origin',(0.,0.,0.));
#12891=CARTESIAN_POINT('',(-0.335,0.0149999999999999,-4.10256677714363E-17));
#12892=CARTESIAN_POINT('Origin',(0.22,0.,0.));
#12893=CARTESIAN_POINT('',(-0.22,-6.93889390390723E-18,-2.69422295812418E-17));
#12894=CARTESIAN_POINT('Origin',(0.,0.,0.));
#12895=CARTESIAN_POINT('Origin',(0.,-0.02,0.));
#12896=CARTESIAN_POINT('',(-0.1954,-0.0492,2.39295984553393E-17));
#12897=CARTESIAN_POINT('Origin',(0.,-0.0492,0.));
#12898=CARTESIAN_POINT('',(-0.21,-0.02,-2.57175827820944E-17));
#12899=CARTESIAN_POINT('Origin',(0.,-0.8,0.));
#12900=CARTESIAN_POINT('',(-0.1954,-1.5646,2.39295984553393E-17));
#12901=CARTESIAN_POINT('Origin',(0.,-1.5646,0.));
#12902=CARTESIAN_POINT('',(-0.1954,-0.8,-2.39295984553393E-17));
#12903=CARTESIAN_POINT('Origin',(0.,-1.58,0.));
#12904=CARTESIAN_POINT('',(-0.16,-1.6,-1.95943487863577E-17));
#12905=CARTESIAN_POINT('Origin',(0.,-1.6,0.));
#12906=CARTESIAN_POINT('',(-0.18,-1.58,-2.20436423846524E-17));
#12907=CARTESIAN_POINT('Origin',(0.,-1.6,0.));
#12908=CARTESIAN_POINT('Origin',(0.0866025403784439,-0.4,-0.15));
#12909=CARTESIAN_POINT('',(0.173205080756888,-0.4,0.));
#12910=CARTESIAN_POINT('',(0.0866025403784439,-0.4,-0.15));
#12911=CARTESIAN_POINT('',(0.173205080756888,-0.4,0.));
#12912=CARTESIAN_POINT('',(0.0866025403784439,-0.64,-0.15));
#12913=CARTESIAN_POINT('',(0.0866025403784439,-0.4,-0.15));
#12914=CARTESIAN_POINT('',(0.173205080756888,-0.64,0.));
#12915=CARTESIAN_POINT('',(0.173205080756888,-0.64,0.));
#12916=CARTESIAN_POINT('',(0.173205080756888,-0.4,0.));
#12917=CARTESIAN_POINT('Origin',(-0.0866025403784438,-0.4,-0.15));
#12918=CARTESIAN_POINT('',(-0.0866025403784438,-0.4,-0.15));
#12919=CARTESIAN_POINT('',(0.0866025403784439,-0.4,-0.15));
#12920=CARTESIAN_POINT('',(-0.0866025403784438,-0.64,-0.15));
#12921=CARTESIAN_POINT('',(-0.0866025403784438,-0.4,-0.15));
#12922=CARTESIAN_POINT('',(0.0866025403784439,-0.64,-0.15));
#12923=CARTESIAN_POINT('Origin',(-0.173205080756888,-0.4,-2.77555756156289E-17));
#12924=CARTESIAN_POINT('',(-0.173205080756888,-0.4,-2.12115047744981E-17));
#12925=CARTESIAN_POINT('',(-0.0866025403784438,-0.4,-0.15));
#12926=CARTESIAN_POINT('',(-0.173205080756888,-0.64,-2.77555756156289E-17));
#12927=CARTESIAN_POINT('',(-0.173205080756888,-0.4,-2.12115047744981E-17));
#12928=CARTESIAN_POINT('',(-0.0866025403784438,-0.64,-0.15));
#12929=CARTESIAN_POINT('Origin',(-0.0866025403784439,-0.4,0.15));
#12930=CARTESIAN_POINT('',(-0.0866025403784439,-0.4,0.15));
#12931=CARTESIAN_POINT('',(-0.173205080756888,-0.4,-2.12115047744981E-17));
#12932=CARTESIAN_POINT('',(-0.0866025403784439,-0.64,0.15));
#12933=CARTESIAN_POINT('',(-0.0866025403784439,-0.4,0.15));
#12934=CARTESIAN_POINT('',(-0.173205080756888,-0.64,-2.12115047744981E-17));
#12935=CARTESIAN_POINT('Origin',(0.0866025403784439,-0.4,0.15));
#12936=CARTESIAN_POINT('',(0.0866025403784439,-0.4,0.15));
#12937=CARTESIAN_POINT('',(-0.0866025403784439,-0.4,0.15));
#12938=CARTESIAN_POINT('',(0.0866025403784439,-0.64,0.15));
#12939=CARTESIAN_POINT('',(0.0866025403784439,-0.4,0.15));
#12940=CARTESIAN_POINT('',(-0.0866025403784439,-0.64,0.15));
#12941=CARTESIAN_POINT('Origin',(0.173205080756888,-0.4,0.));
#12942=CARTESIAN_POINT('',(0.0866025403784439,-0.4,0.15));
#12943=CARTESIAN_POINT('',(0.0866025403784439,-0.64,0.15));
#12944=CARTESIAN_POINT('Origin',(0.,-0.4,-2.77555756156289E-17));
#12945=CARTESIAN_POINT('Origin',(0.,-0.64,-2.77555756156289E-17));
#12946=CARTESIAN_POINT('',(0.,0.,0.));
#12947=CARTESIAN_POINT('',(0.,0.,0.));
#12948=CARTESIAN_POINT('',(0.,0.,0.));
#12949=CARTESIAN_POINT('',(0.,0.,0.));
#12950=CARTESIAN_POINT('',(0.,0.,0.));
#12951=CARTESIAN_POINT('',(0.,0.,0.));
#12952=CARTESIAN_POINT('',(0.,0.,0.));
#12953=CARTESIAN_POINT('',(0.,0.,0.));
#12954=CARTESIAN_POINT('',(0.,0.,0.));
#12955=CARTESIAN_POINT('',(0.,0.,0.));
#12956=CARTESIAN_POINT('',(0.,0.,0.));
#12957=CARTESIAN_POINT('',(0.,0.,0.));
#12958=CARTESIAN_POINT('',(0.,0.,0.));
#12959=CARTESIAN_POINT('',(0.,0.,0.));
#12960=CARTESIAN_POINT('',(0.,0.,0.));
#12961=CARTESIAN_POINT('',(0.,0.,0.));
#12962=CARTESIAN_POINT('',(0.,0.,0.));
#12963=CARTESIAN_POINT('',(0.,0.,0.));
#12964=CARTESIAN_POINT('',(0.,0.,0.));
#12965=CARTESIAN_POINT('',(3.,-11.,0.));
#12966=CARTESIAN_POINT('',(3.,-11.,-1.));
#12967=CARTESIAN_POINT('',(3.,-11.,41.));
#12968=CARTESIAN_POINT('',(3.,11.,0.));
#12969=CARTESIAN_POINT('',(3.,11.,-1.));
#12970=CARTESIAN_POINT('',(3.,11.,41.));
#12971=CARTESIAN_POINT('',(23.,-11.,0.));
#12972=CARTESIAN_POINT('',(23.,-11.,-1.));
#12973=CARTESIAN_POINT('',(23.,-11.,41.));
#12974=CARTESIAN_POINT('',(23.,11.,0.));
#12975=CARTESIAN_POINT('',(23.,11.,-1.));
#12976=CARTESIAN_POINT('',(23.,11.,41.));
#12977=CARTESIAN_POINT('',(3.,-10.58,7.));
#12978=CARTESIAN_POINT('',(3.,-8.5,7.));
#12979=CARTESIAN_POINT('',(2.3,-7.5,7.));
#12980=CARTESIAN_POINT('',(3.,10.58,7.));
#12981=CARTESIAN_POINT('',(3.,8.5,7.));
#12982=CARTESIAN_POINT('',(2.3,7.5,7.));
#12983=CARTESIAN_POINT('',(23.,-10.58,12.));
#12984=CARTESIAN_POINT('',(23.,-8.5,12.));
#12985=CARTESIAN_POINT('',(22.3,-7.5,12.));
#12986=CARTESIAN_POINT('',(23.,10.58,12.));
#12987=CARTESIAN_POINT('',(23.,8.5,12.));
#12988=CARTESIAN_POINT('',(22.3,7.5,12.));
#12989=CARTESIAN_POINT('',(2.58,11.,6.));
#12990=CARTESIAN_POINT('',(1.2,11.,6.));
#12991=CARTESIAN_POINT('',(1.1,11.,6.));
#12992=CARTESIAN_POINT('',(2.58,11.,31.5));
#12993=CARTESIAN_POINT('',(1.2,11.,31.5));
#12994=CARTESIAN_POINT('',(1.1,11.,31.5));
#12995=CARTESIAN_POINT('',(1.2,11.,7.5));
#12996=CARTESIAN_POINT('',(0.23,11.,9.5));
#12997=CARTESIAN_POINT('',(0.23,11.,15.5));
#12998=CARTESIAN_POINT('',(0.23,11.,21.5));
#12999=CARTESIAN_POINT('',(0.23,11.,27.5));
#13000=CARTESIAN_POINT('',(2.58,-11.,19.));
#13001=CARTESIAN_POINT('',(1.2,-11.,19.));
#13002=CARTESIAN_POINT('',(1.1,-11.,19.));
#13003=CARTESIAN_POINT('',(-2.,-8.4,18.3));
#13004=CARTESIAN_POINT('',(2.58,-11.,31.));
#13005=CARTESIAN_POINT('',(1.2,-11.,31.));
#13006=CARTESIAN_POINT('',(1.1,-11.,31.));
#13007=CARTESIAN_POINT('',(-2.,-8.4,30.3));
#13008=CARTESIAN_POINT('',(-1.4,11.,6.95));
#13009=CARTESIAN_POINT('',(-1.4,11.,30.25));
#13010=CARTESIAN_POINT('',(0.,0.,0.));
#13011=CARTESIAN_POINT('',(0.,0.,0.));
#13012=CARTESIAN_POINT('',(1.2,11.,11.));
#13013=CARTESIAN_POINT('',(-1.6,9.1,9.5));
#13014=CARTESIAN_POINT('',(-1.6,9.1,12.5));
#13015=CARTESIAN_POINT('',(-1.6,12.9,9.5));
#13016=CARTESIAN_POINT('',(-1.6,12.9,12.5));
#13017=CARTESIAN_POINT('',(-1.2,-2.5,15.));
#13018=CARTESIAN_POINT('',(-1.2,2.5,15.));
#13019=CARTESIAN_POINT('',(0.,0.,0.));
#13020=CARTESIAN_POINT('',(0.,0.,0.));
#13021=UNCERTAINTY_MEASURE_WITH_UNIT(LENGTH_MEASURE(0.001),#13095,
'DISTANCE_ACCURACY_VALUE',
'Maximum model space distance between geometric entities at asserted c
onnectivities');
#13022=UNCERTAINTY_MEASURE_WITH_UNIT(LENGTH_MEASURE(0.001),#13095,
'DISTANCE_ACCURACY_VALUE',
'Maximum model space distance between geometric entities at asserted c
onnectivities');
#13023=UNCERTAINTY_MEASURE_WITH_UNIT(LENGTH_MEASURE(0.001),#13095,
'DISTANCE_ACCURACY_VALUE',
'Maximum model space distance between geometric entities at asserted c
onnectivities');
#13024=UNCERTAINTY_MEASURE_WITH_UNIT(LENGTH_MEASURE(0.001),#13095,
'DISTANCE_ACCURACY_VALUE',
'Maximum model space distance between geometric entities at asserted c
onnectivities');
#13025=UNCERTAINTY_MEASURE_WITH_UNIT(LENGTH_MEASURE(0.001),#13095,
'DISTANCE_ACCURACY_VALUE',
'Maximum model space distance between geometric entities at asserted c
onnectivities');
#13026=UNCERTAINTY_MEASURE_WITH_UNIT(LENGTH_MEASURE(0.001),#13095,
'DISTANCE_ACCURACY_VALUE',
'Maximum model space distance between geometric entities at asserted c
onnectivities');
#13027=UNCERTAINTY_MEASURE_WITH_UNIT(LENGTH_MEASURE(0.001),#13095,
'DISTANCE_ACCURACY_VALUE',
'Maximum model space distance between geometric entities at asserted c
onnectivities');
#13028=UNCERTAINTY_MEASURE_WITH_UNIT(LENGTH_MEASURE(0.001),#13095,
'DISTANCE_ACCURACY_VALUE',
'Maximum model space distance between geometric entities at asserted c
onnectivities');
#13029=UNCERTAINTY_MEASURE_WITH_UNIT(LENGTH_MEASURE(0.001),#13095,
'DISTANCE_ACCURACY_VALUE',
'Maximum model space distance between geometric entities at asserted c
onnectivities');
#13030=UNCERTAINTY_MEASURE_WITH_UNIT(LENGTH_MEASURE(0.001),#13095,
'DISTANCE_ACCURACY_VALUE',
'Maximum model space distance between geometric entities at asserted c
onnectivities');
#13031=UNCERTAINTY_MEASURE_WITH_UNIT(LENGTH_MEASURE(0.001),#13095,
'DISTANCE_ACCURACY_VALUE',
'Maximum model space distance between geometric entities at asserted c
onnectivities');
#13032=UNCERTAINTY_MEASURE_WITH_UNIT(LENGTH_MEASURE(0.001),#13095,
'DISTANCE_ACCURACY_VALUE',
'Maximum model space distance between geometric entities at asserted c
onnectivities');
#13033=UNCERTAINTY_MEASURE_WITH_UNIT(LENGTH_MEASURE(0.001),#13095,
'DISTANCE_ACCURACY_VALUE',
'Maximum model space distance between geometric entities at asserted c
onnectivities');
#13034=UNCERTAINTY_MEASURE_WITH_UNIT(LENGTH_MEASURE(0.001),#13095,
'DISTANCE_ACCURACY_VALUE',
'Maximum model space distance between geometric entities at asserted c
onnectivities');
#13035=UNCERTAINTY_MEASURE_WITH_UNIT(LENGTH_MEASURE(0.001),#13095,
'DISTANCE_ACCURACY_VALUE',
'Maximum model space distance between geometric entities at asserted c
onnectivities');
#13036=UNCERTAINTY_MEASURE_WITH_UNIT(LENGTH_MEASURE(0.001),#13095,
'DISTANCE_ACCURACY_VALUE',
'Maximum model space distance between geometric entities at asserted c
onnectivities');
#13037=UNCERTAINTY_MEASURE_WITH_UNIT(LENGTH_MEASURE(0.001),#13095,
'DISTANCE_ACCURACY_VALUE',
'Maximum model space distance between geometric entities at asserted c
onnectivities');
#13038=UNCERTAINTY_MEASURE_WITH_UNIT(LENGTH_MEASURE(0.001),#13095,
'DISTANCE_ACCURACY_VALUE',
'Maximum model space distance between geometric entities at asserted c
onnectivities');
#13039=UNCERTAINTY_MEASURE_WITH_UNIT(LENGTH_MEASURE(0.001),#13095,
'DISTANCE_ACCURACY_VALUE',
'Maximum model space distance between geometric entities at asserted c
onnectivities');
#13040=UNCERTAINTY_MEASURE_WITH_UNIT(LENGTH_MEASURE(0.001),#13095,
'DISTANCE_ACCURACY_VALUE',
'Maximum model space distance between geometric entities at asserted c
onnectivities');
#13041=UNCERTAINTY_MEASURE_WITH_UNIT(LENGTH_MEASURE(0.001),#13095,
'DISTANCE_ACCURACY_VALUE',
'Maximum model space distance between geometric entities at asserted c
onnectivities');
#13042=UNCERTAINTY_MEASURE_WITH_UNIT(LENGTH_MEASURE(0.001),#13095,
'DISTANCE_ACCURACY_VALUE',
'Maximum model space distance between geometric entities at asserted c
onnectivities');
#13043=UNCERTAINTY_MEASURE_WITH_UNIT(LENGTH_MEASURE(0.001),#13095,
'DISTANCE_ACCURACY_VALUE',
'Maximum model space distance between geometric entities at asserted c
onnectivities');
#13044=UNCERTAINTY_MEASURE_WITH_UNIT(LENGTH_MEASURE(0.001),#13095,
'DISTANCE_ACCURACY_VALUE',
'Maximum model space distance between geometric entities at asserted c
onnectivities');
#13045=UNCERTAINTY_MEASURE_WITH_UNIT(LENGTH_MEASURE(0.001),#13095,
'DISTANCE_ACCURACY_VALUE',
'Maximum model space distance between geometric entities at asserted c
onnectivities');
#13046=UNCERTAINTY_MEASURE_WITH_UNIT(LENGTH_MEASURE(0.001),#13095,
'DISTANCE_ACCURACY_VALUE',
'Maximum model space distance between geometric entities at asserted c
onnectivities');
#13047=UNCERTAINTY_MEASURE_WITH_UNIT(LENGTH_MEASURE(0.001),#13095,
'DISTANCE_ACCURACY_VALUE',
'Maximum model space distance between geometric entities at asserted c
onnectivities');
#13048=UNCERTAINTY_MEASURE_WITH_UNIT(LENGTH_MEASURE(0.001),#13095,
'DISTANCE_ACCURACY_VALUE',
'Maximum model space distance between geometric entities at asserted c
onnectivities');
#13049=UNCERTAINTY_MEASURE_WITH_UNIT(LENGTH_MEASURE(0.001),#13095,
'DISTANCE_ACCURACY_VALUE',
'Maximum model space distance between geometric entities at asserted c
onnectivities');
#13050=UNCERTAINTY_MEASURE_WITH_UNIT(LENGTH_MEASURE(0.001),#13095,
'DISTANCE_ACCURACY_VALUE',
'Maximum model space distance between geometric entities at asserted c
onnectivities');
#13051=UNCERTAINTY_MEASURE_WITH_UNIT(LENGTH_MEASURE(0.001),#13095,
'DISTANCE_ACCURACY_VALUE',
'Maximum model space distance between geometric entities at asserted c
onnectivities');
#13052=UNCERTAINTY_MEASURE_WITH_UNIT(LENGTH_MEASURE(0.001),#13095,
'DISTANCE_ACCURACY_VALUE',
'Maximum model space distance between geometric entities at asserted c
onnectivities');
#13053=UNCERTAINTY_MEASURE_WITH_UNIT(LENGTH_MEASURE(0.001),#13095,
'DISTANCE_ACCURACY_VALUE',
'Maximum model space distance between geometric entities at asserted c
onnectivities');
#13054=UNCERTAINTY_MEASURE_WITH_UNIT(LENGTH_MEASURE(0.001),#13095,
'DISTANCE_ACCURACY_VALUE',
'Maximum model space distance between geometric entities at asserted c
onnectivities');
#13055=UNCERTAINTY_MEASURE_WITH_UNIT(LENGTH_MEASURE(0.001),#13095,
'DISTANCE_ACCURACY_VALUE',
'Maximum model space distance between geometric entities at asserted c
onnectivities');
#13056=UNCERTAINTY_MEASURE_WITH_UNIT(LENGTH_MEASURE(0.001),#13095,
'DISTANCE_ACCURACY_VALUE',
'Maximum model space distance between geometric entities at asserted c
onnectivities');
#13057=UNCERTAINTY_MEASURE_WITH_UNIT(LENGTH_MEASURE(0.001),#13095,
'DISTANCE_ACCURACY_VALUE',
'Maximum model space distance between geometric entities at asserted c
onnectivities');
#13058=(
GEOMETRIC_REPRESENTATION_CONTEXT(3)
GLOBAL_UNCERTAINTY_ASSIGNED_CONTEXT((#13021))
GLOBAL_UNIT_ASSIGNED_CONTEXT((#13095,#13097,#13098))
REPRESENTATION_CONTEXT('','3D')
);
#13059=(
GEOMETRIC_REPRESENTATION_CONTEXT(3)
GLOBAL_UNCERTAINTY_ASSIGNED_CONTEXT((#13022))
GLOBAL_UNIT_ASSIGNED_CONTEXT((#13095,#13097,#13098))
REPRESENTATION_CONTEXT('','3D')
);
#13060=(
GEOMETRIC_REPRESENTATION_CONTEXT(3)
GLOBAL_UNCERTAINTY_ASSIGNED_CONTEXT((#13023))
GLOBAL_UNIT_ASSIGNED_CONTEXT((#13095,#13097,#13098))
REPRESENTATION_CONTEXT('','3D')
);
#13061=(
GEOMETRIC_REPRESENTATION_CONTEXT(3)
GLOBAL_UNCERTAINTY_ASSIGNED_CONTEXT((#13024))
GLOBAL_UNIT_ASSIGNED_CONTEXT((#13095,#13097,#13098))
REPRESENTATION_CONTEXT('','3D')
);
#13062=(
GEOMETRIC_REPRESENTATION_CONTEXT(3)
GLOBAL_UNCERTAINTY_ASSIGNED_CONTEXT((#13025))
GLOBAL_UNIT_ASSIGNED_CONTEXT((#13095,#13097,#13098))
REPRESENTATION_CONTEXT('','3D')
);
#13063=(
GEOMETRIC_REPRESENTATION_CONTEXT(3)
GLOBAL_UNCERTAINTY_ASSIGNED_CONTEXT((#13026))
GLOBAL_UNIT_ASSIGNED_CONTEXT((#13095,#13097,#13098))
REPRESENTATION_CONTEXT('','3D')
);
#13064=(
GEOMETRIC_REPRESENTATION_CONTEXT(3)
GLOBAL_UNCERTAINTY_ASSIGNED_CONTEXT((#13027))
GLOBAL_UNIT_ASSIGNED_CONTEXT((#13095,#13097,#13098))
REPRESENTATION_CONTEXT('','3D')
);
#13065=(
GEOMETRIC_REPRESENTATION_CONTEXT(3)
GLOBAL_UNCERTAINTY_ASSIGNED_CONTEXT((#13028))
GLOBAL_UNIT_ASSIGNED_CONTEXT((#13095,#13097,#13098))
REPRESENTATION_CONTEXT('','3D')
);
#13066=(
GEOMETRIC_REPRESENTATION_CONTEXT(3)
GLOBAL_UNCERTAINTY_ASSIGNED_CONTEXT((#13029))
GLOBAL_UNIT_ASSIGNED_CONTEXT((#13095,#13097,#13098))
REPRESENTATION_CONTEXT('','3D')
);
#13067=(
GEOMETRIC_REPRESENTATION_CONTEXT(3)
GLOBAL_UNCERTAINTY_ASSIGNED_CONTEXT((#13030))
GLOBAL_UNIT_ASSIGNED_CONTEXT((#13095,#13097,#13098))
REPRESENTATION_CONTEXT('','3D')
);
#13068=(
GEOMETRIC_REPRESENTATION_CONTEXT(3)
GLOBAL_UNCERTAINTY_ASSIGNED_CONTEXT((#13031))
GLOBAL_UNIT_ASSIGNED_CONTEXT((#13095,#13097,#13098))
REPRESENTATION_CONTEXT('','3D')
);
#13069=(
GEOMETRIC_REPRESENTATION_CONTEXT(3)
GLOBAL_UNCERTAINTY_ASSIGNED_CONTEXT((#13032))
GLOBAL_UNIT_ASSIGNED_CONTEXT((#13095,#13097,#13098))
REPRESENTATION_CONTEXT('','3D')
);
#13070=(
GEOMETRIC_REPRESENTATION_CONTEXT(3)
GLOBAL_UNCERTAINTY_ASSIGNED_CONTEXT((#13033))
GLOBAL_UNIT_ASSIGNED_CONTEXT((#13095,#13097,#13098))
REPRESENTATION_CONTEXT('','3D')
);
#13071=(
GEOMETRIC_REPRESENTATION_CONTEXT(3)
GLOBAL_UNCERTAINTY_ASSIGNED_CONTEXT((#13034))
GLOBAL_UNIT_ASSIGNED_CONTEXT((#13095,#13097,#13098))
REPRESENTATION_CONTEXT('','3D')
);
#13072=(
GEOMETRIC_REPRESENTATION_CONTEXT(3)
GLOBAL_UNCERTAINTY_ASSIGNED_CONTEXT((#13035))
GLOBAL_UNIT_ASSIGNED_CONTEXT((#13095,#13097,#13098))
REPRESENTATION_CONTEXT('','3D')
);
#13073=(
GEOMETRIC_REPRESENTATION_CONTEXT(3)
GLOBAL_UNCERTAINTY_ASSIGNED_CONTEXT((#13036))
GLOBAL_UNIT_ASSIGNED_CONTEXT((#13095,#13097,#13098))
REPRESENTATION_CONTEXT('','3D')
);
#13074=(
GEOMETRIC_REPRESENTATION_CONTEXT(3)
GLOBAL_UNCERTAINTY_ASSIGNED_CONTEXT((#13037))
GLOBAL_UNIT_ASSIGNED_CONTEXT((#13095,#13097,#13098))
REPRESENTATION_CONTEXT('','3D')
);
#13075=(
GEOMETRIC_REPRESENTATION_CONTEXT(3)
GLOBAL_UNCERTAINTY_ASSIGNED_CONTEXT((#13038))
GLOBAL_UNIT_ASSIGNED_CONTEXT((#13095,#13097,#13098))
REPRESENTATION_CONTEXT('','3D')
);
#13076=(
GEOMETRIC_REPRESENTATION_CONTEXT(3)
GLOBAL_UNCERTAINTY_ASSIGNED_CONTEXT((#13039))
GLOBAL_UNIT_ASSIGNED_CONTEXT((#13095,#13097,#13098))
REPRESENTATION_CONTEXT('','3D')
);
#13077=(
GEOMETRIC_REPRESENTATION_CONTEXT(3)
GLOBAL_UNCERTAINTY_ASSIGNED_CONTEXT((#13040))
GLOBAL_UNIT_ASSIGNED_CONTEXT((#13095,#13097,#13098))
REPRESENTATION_CONTEXT('','3D')
);
#13078=(
GEOMETRIC_REPRESENTATION_CONTEXT(3)
GLOBAL_UNCERTAINTY_ASSIGNED_CONTEXT((#13041))
GLOBAL_UNIT_ASSIGNED_CONTEXT((#13095,#13097,#13098))
REPRESENTATION_CONTEXT('','3D')
);
#13079=(
GEOMETRIC_REPRESENTATION_CONTEXT(3)
GLOBAL_UNCERTAINTY_ASSIGNED_CONTEXT((#13042))
GLOBAL_UNIT_ASSIGNED_CONTEXT((#13095,#13097,#13098))
REPRESENTATION_CONTEXT('','3D')
);
#13080=(
GEOMETRIC_REPRESENTATION_CONTEXT(3)
GLOBAL_UNCERTAINTY_ASSIGNED_CONTEXT((#13043))
GLOBAL_UNIT_ASSIGNED_CONTEXT((#13095,#13097,#13098))
REPRESENTATION_CONTEXT('','3D')
);
#13081=(
GEOMETRIC_REPRESENTATION_CONTEXT(3)
GLOBAL_UNCERTAINTY_ASSIGNED_CONTEXT((#13044))
GLOBAL_UNIT_ASSIGNED_CONTEXT((#13095,#13097,#13098))
REPRESENTATION_CONTEXT('','3D')
);
#13082=(
GEOMETRIC_REPRESENTATION_CONTEXT(3)
GLOBAL_UNCERTAINTY_ASSIGNED_CONTEXT((#13045))
GLOBAL_UNIT_ASSIGNED_CONTEXT((#13095,#13097,#13098))
REPRESENTATION_CONTEXT('','3D')
);
#13083=(
GEOMETRIC_REPRESENTATION_CONTEXT(3)
GLOBAL_UNCERTAINTY_ASSIGNED_CONTEXT((#13046))
GLOBAL_UNIT_ASSIGNED_CONTEXT((#13095,#13097,#13098))
REPRESENTATION_CONTEXT('','3D')
);
#13084=(
GEOMETRIC_REPRESENTATION_CONTEXT(3)
GLOBAL_UNCERTAINTY_ASSIGNED_CONTEXT((#13047))
GLOBAL_UNIT_ASSIGNED_CONTEXT((#13095,#13097,#13098))
REPRESENTATION_CONTEXT('','3D')
);
#13085=(
GEOMETRIC_REPRESENTATION_CONTEXT(3)
GLOBAL_UNCERTAINTY_ASSIGNED_CONTEXT((#13048))
GLOBAL_UNIT_ASSIGNED_CONTEXT((#13095,#13097,#13098))
REPRESENTATION_CONTEXT('','3D')
);
#13086=(
GEOMETRIC_REPRESENTATION_CONTEXT(3)
GLOBAL_UNCERTAINTY_ASSIGNED_CONTEXT((#13049))
GLOBAL_UNIT_ASSIGNED_CONTEXT((#13095,#13097,#13098))
REPRESENTATION_CONTEXT('','3D')
);
#13087=(
GEOMETRIC_REPRESENTATION_CONTEXT(3)
GLOBAL_UNCERTAINTY_ASSIGNED_CONTEXT((#13050))
GLOBAL_UNIT_ASSIGNED_CONTEXT((#13095,#13097,#13098))
REPRESENTATION_CONTEXT('','3D')
);
#13088=(
GEOMETRIC_REPRESENTATION_CONTEXT(3)
GLOBAL_UNCERTAINTY_ASSIGNED_CONTEXT((#13051))
GLOBAL_UNIT_ASSIGNED_CONTEXT((#13095,#13097,#13098))
REPRESENTATION_CONTEXT('','3D')
);
#13089=(
GEOMETRIC_REPRESENTATION_CONTEXT(3)
GLOBAL_UNCERTAINTY_ASSIGNED_CONTEXT((#13052))
GLOBAL_UNIT_ASSIGNED_CONTEXT((#13095,#13097,#13098))
REPRESENTATION_CONTEXT('','3D')
);
#13090=(
GEOMETRIC_REPRESENTATION_CONTEXT(3)
GLOBAL_UNCERTAINTY_ASSIGNED_CONTEXT((#13053))
GLOBAL_UNIT_ASSIGNED_CONTEXT((#13095,#13097,#13098))
REPRESENTATION_CONTEXT('','3D')
);
#13091=(
GEOMETRIC_REPRESENTATION_CONTEXT(3)
GLOBAL_UNCERTAINTY_ASSIGNED_CONTEXT((#13054))
GLOBAL_UNIT_ASSIGNED_CONTEXT((#13095,#13097,#13098))
REPRESENTATION_CONTEXT('','3D')
);
#13092=(
GEOMETRIC_REPRESENTATION_CONTEXT(3)
GLOBAL_UNCERTAINTY_ASSIGNED_CONTEXT((#13055))
GLOBAL_UNIT_ASSIGNED_CONTEXT((#13095,#13097,#13098))
REPRESENTATION_CONTEXT('','3D')
);
#13093=(
GEOMETRIC_REPRESENTATION_CONTEXT(3)
GLOBAL_UNCERTAINTY_ASSIGNED_CONTEXT((#13056))
GLOBAL_UNIT_ASSIGNED_CONTEXT((#13095,#13097,#13098))
REPRESENTATION_CONTEXT('','3D')
);
#13094=(
GEOMETRIC_REPRESENTATION_CONTEXT(3)
GLOBAL_UNCERTAINTY_ASSIGNED_CONTEXT((#13057))
GLOBAL_UNIT_ASSIGNED_CONTEXT((#13095,#13097,#13098))
REPRESENTATION_CONTEXT('','3D')
);
#13095=(
LENGTH_UNIT()
NAMED_UNIT(*)
SI_UNIT(.CENTI.,.METRE.)
);
#13096=(
LENGTH_UNIT()
NAMED_UNIT(*)
SI_UNIT($,.METRE.)
);
#13097=(
NAMED_UNIT(*)
PLANE_ANGLE_UNIT()
SI_UNIT($,.RADIAN.)
);
#13098=(
NAMED_UNIT(*)
SI_UNIT($,.STERADIAN.)
SOLID_ANGLE_UNIT()
);
#13099=SHAPE_DEFINITION_REPRESENTATION(#13135,#13249);
#13100=SHAPE_DEFINITION_REPRESENTATION(#13136,#13250);
#13101=SHAPE_DEFINITION_REPRESENTATION(#13137,#13251);
#13102=SHAPE_DEFINITION_REPRESENTATION(#13138,#13252);
#13103=SHAPE_DEFINITION_REPRESENTATION(#13139,#13253);
#13104=SHAPE_DEFINITION_REPRESENTATION(#13140,#13254);
#13105=SHAPE_DEFINITION_REPRESENTATION(#13141,#13255);
#13106=SHAPE_DEFINITION_REPRESENTATION(#13142,#13256);
#13107=SHAPE_DEFINITION_REPRESENTATION(#13143,#13257);
#13108=SHAPE_DEFINITION_REPRESENTATION(#13144,#13258);
#13109=SHAPE_DEFINITION_REPRESENTATION(#13145,#13259);
#13110=SHAPE_DEFINITION_REPRESENTATION(#13146,#13260);
#13111=SHAPE_DEFINITION_REPRESENTATION(#13147,#13261);
#13112=SHAPE_DEFINITION_REPRESENTATION(#13148,#13262);
#13113=SHAPE_DEFINITION_REPRESENTATION(#13149,#13263);
#13114=SHAPE_DEFINITION_REPRESENTATION(#13150,#13264);
#13115=SHAPE_DEFINITION_REPRESENTATION(#13151,#13265);
#13116=SHAPE_DEFINITION_REPRESENTATION(#13152,#13266);
#13117=SHAPE_DEFINITION_REPRESENTATION(#13153,#13267);
#13118=SHAPE_DEFINITION_REPRESENTATION(#13154,#13268);
#13119=SHAPE_DEFINITION_REPRESENTATION(#13155,#13269);
#13120=SHAPE_DEFINITION_REPRESENTATION(#13156,#13270);
#13121=SHAPE_DEFINITION_REPRESENTATION(#13157,#13271);
#13122=SHAPE_DEFINITION_REPRESENTATION(#13158,#13272);
#13123=SHAPE_DEFINITION_REPRESENTATION(#13159,#13273);
#13124=SHAPE_DEFINITION_REPRESENTATION(#13160,#13274);
#13125=SHAPE_DEFINITION_REPRESENTATION(#13161,#13275);
#13126=SHAPE_DEFINITION_REPRESENTATION(#13162,#13276);
#13127=SHAPE_DEFINITION_REPRESENTATION(#13163,#13277);
#13128=SHAPE_DEFINITION_REPRESENTATION(#13164,#13278);
#13129=SHAPE_DEFINITION_REPRESENTATION(#13165,#13279);
#13130=SHAPE_DEFINITION_REPRESENTATION(#13166,#13280);
#13131=SHAPE_DEFINITION_REPRESENTATION(#13167,#13281);
#13132=SHAPE_DEFINITION_REPRESENTATION(#13168,#13282);
#13133=SHAPE_DEFINITION_REPRESENTATION(#13172,#13283);
#13134=SHAPE_DEFINITION_REPRESENTATION(#13173,#13284);
#13135=PRODUCT_DEFINITION_SHAPE('',$,#13286);
#13136=PRODUCT_DEFINITION_SHAPE('',$,#13287);
#13137=PRODUCT_DEFINITION_SHAPE('',$,#13288);
#13138=PRODUCT_DEFINITION_SHAPE('',$,#13289);
#13139=PRODUCT_DEFINITION_SHAPE('',$,#13290);
#13140=PRODUCT_DEFINITION_SHAPE('',$,#13291);
#13141=PRODUCT_DEFINITION_SHAPE('',$,#13292);
#13142=PRODUCT_DEFINITION_SHAPE('',$,#13293);
#13143=PRODUCT_DEFINITION_SHAPE('',$,#13294);
#13144=PRODUCT_DEFINITION_SHAPE('',$,#13295);
#13145=PRODUCT_DEFINITION_SHAPE('',$,#13296);
#13146=PRODUCT_DEFINITION_SHAPE('',$,#13297);
#13147=PRODUCT_DEFINITION_SHAPE('',$,#13298);
#13148=PRODUCT_DEFINITION_SHAPE('',$,#13299);
#13149=PRODUCT_DEFINITION_SHAPE('',$,#13300);
#13150=PRODUCT_DEFINITION_SHAPE('',$,#13301);
#13151=PRODUCT_DEFINITION_SHAPE('',$,#13302);
#13152=PRODUCT_DEFINITION_SHAPE('',$,#13303);
#13153=PRODUCT_DEFINITION_SHAPE('',$,#13304);
#13154=PRODUCT_DEFINITION_SHAPE('',$,#13305);
#13155=PRODUCT_DEFINITION_SHAPE('',$,#13306);
#13156=PRODUCT_DEFINITION_SHAPE('',$,#13307);
#13157=PRODUCT_DEFINITION_SHAPE('',$,#13308);
#13158=PRODUCT_DEFINITION_SHAPE('',$,#13309);
#13159=PRODUCT_DEFINITION_SHAPE('',$,#13310);
#13160=PRODUCT_DEFINITION_SHAPE('',$,#13311);
#13161=PRODUCT_DEFINITION_SHAPE('',$,#13312);
#13162=PRODUCT_DEFINITION_SHAPE('',$,#13313);
#13163=PRODUCT_DEFINITION_SHAPE('',$,#13314);
#13164=PRODUCT_DEFINITION_SHAPE('',$,#13315);
#13165=PRODUCT_DEFINITION_SHAPE('',$,#13316);
#13166=PRODUCT_DEFINITION_SHAPE('',$,#13317);
#13167=PRODUCT_DEFINITION_SHAPE('',$,#13318);
#13168=PRODUCT_DEFINITION_SHAPE('',$,#13319);
#13169=PRODUCT_DEFINITION_SHAPE($,$,#245);
#13170=PRODUCT_DEFINITION_SHAPE($,$,#246);
#13171=PRODUCT_DEFINITION_SHAPE($,$,#247);
#13172=PRODUCT_DEFINITION_SHAPE('',$,#13320);
#13173=PRODUCT_DEFINITION_SHAPE('',$,#13321);
#13174=PRODUCT_DEFINITION_SHAPE($,$,#248);
#13175=PRODUCT_DEFINITION_SHAPE($,$,#249);
#13176=PRODUCT_DEFINITION_SHAPE($,$,#250);
#13177=PRODUCT_DEFINITION_SHAPE($,$,#251);
#13178=PRODUCT_DEFINITION_SHAPE($,$,#252);
#13179=PRODUCT_DEFINITION_SHAPE($,$,#253);
#13180=PRODUCT_DEFINITION_SHAPE($,$,#254);
#13181=PRODUCT_DEFINITION_SHAPE($,$,#255);
#13182=PRODUCT_DEFINITION_SHAPE($,$,#256);
#13183=PRODUCT_DEFINITION_SHAPE($,$,#257);
#13184=PRODUCT_DEFINITION_SHAPE($,$,#258);
#13185=PRODUCT_DEFINITION_SHAPE($,$,#259);
#13186=PRODUCT_DEFINITION_SHAPE($,$,#260);
#13187=PRODUCT_DEFINITION_SHAPE($,$,#261);
#13188=PRODUCT_DEFINITION_SHAPE($,$,#262);
#13189=PRODUCT_DEFINITION_SHAPE($,$,#263);
#13190=PRODUCT_DEFINITION_SHAPE($,$,#264);
#13191=PRODUCT_DEFINITION_SHAPE($,$,#265);
#13192=PRODUCT_DEFINITION_SHAPE($,$,#266);
#13193=PRODUCT_DEFINITION_SHAPE($,$,#267);
#13194=PRODUCT_DEFINITION_SHAPE($,$,#268);
#13195=PRODUCT_DEFINITION_SHAPE($,$,#269);
#13196=PRODUCT_DEFINITION_SHAPE($,$,#270);
#13197=PRODUCT_DEFINITION_SHAPE($,$,#271);
#13198=PRODUCT_DEFINITION_SHAPE($,$,#272);
#13199=PRODUCT_DEFINITION_SHAPE($,$,#273);
#13200=PRODUCT_DEFINITION_SHAPE($,$,#274);
#13201=PRODUCT_DEFINITION_SHAPE($,$,#275);
#13202=PRODUCT_DEFINITION_SHAPE($,$,#276);
#13203=PRODUCT_DEFINITION_SHAPE($,$,#277);
#13204=PRODUCT_DEFINITION_SHAPE($,$,#278);
#13205=PRODUCT_DEFINITION_SHAPE($,$,#279);
#13206=PRODUCT_DEFINITION_SHAPE($,$,#280);
#13207=PRODUCT_DEFINITION_SHAPE($,$,#281);
#13208=PRODUCT_DEFINITION_SHAPE($,$,#282);
#13209=PRODUCT_DEFINITION_SHAPE($,$,#283);
#13210=PRODUCT_DEFINITION_SHAPE($,$,#284);
#13211=PRODUCT_DEFINITION_SHAPE($,$,#285);
#13212=PRODUCT_DEFINITION_SHAPE($,$,#286);
#13213=PRODUCT_DEFINITION_SHAPE($,$,#287);
#13214=PRODUCT_DEFINITION_SHAPE($,$,#288);
#13215=PRODUCT_DEFINITION_SHAPE($,$,#289);
#13216=PRODUCT_DEFINITION_SHAPE($,$,#290);
#13217=PRODUCT_DEFINITION_SHAPE($,$,#291);
#13218=PRODUCT_DEFINITION_SHAPE($,$,#292);
#13219=PRODUCT_DEFINITION_SHAPE($,$,#293);
#13220=PRODUCT_DEFINITION_SHAPE($,$,#294);
#13221=PRODUCT_DEFINITION_SHAPE($,$,#295);
#13222=PRODUCT_DEFINITION_SHAPE($,$,#296);
#13223=PRODUCT_DEFINITION_SHAPE($,$,#297);
#13224=PRODUCT_DEFINITION_SHAPE($,$,#298);
#13225=PRODUCT_DEFINITION_SHAPE($,$,#299);
#13226=PRODUCT_DEFINITION_SHAPE($,$,#300);
#13227=PRODUCT_DEFINITION_SHAPE($,$,#301);
#13228=PRODUCT_DEFINITION_SHAPE($,$,#302);
#13229=PRODUCT_DEFINITION_SHAPE($,$,#303);
#13230=PRODUCT_DEFINITION_SHAPE($,$,#304);
#13231=PRODUCT_DEFINITION_SHAPE($,$,#305);
#13232=PRODUCT_DEFINITION_SHAPE($,$,#306);
#13233=PRODUCT_DEFINITION_SHAPE($,$,#307);
#13234=PRODUCT_DEFINITION_SHAPE($,$,#308);
#13235=PRODUCT_DEFINITION_SHAPE($,$,#309);
#13236=PRODUCT_DEFINITION_SHAPE($,$,#310);
#13237=PRODUCT_DEFINITION_SHAPE($,$,#311);
#13238=PRODUCT_DEFINITION_SHAPE($,$,#312);
#13239=PRODUCT_DEFINITION_SHAPE($,$,#313);
#13240=PRODUCT_DEFINITION_SHAPE($,$,#314);
#13241=PRODUCT_DEFINITION_SHAPE($,$,#315);
#13242=PRODUCT_DEFINITION_SHAPE($,$,#316);
#13243=PRODUCT_DEFINITION_SHAPE($,$,#317);
#13244=PRODUCT_DEFINITION_SHAPE($,$,#318);
#13245=PRODUCT_DEFINITION_SHAPE($,$,#319);
#13246=PRODUCT_DEFINITION_SHAPE($,$,#320);
#13247=PRODUCT_DEFINITION_SHAPE($,$,#321);
#13248=PRODUCT_DEFINITION_SHAPE($,$,#322);
#13249=SHAPE_REPRESENTATION('',(#7986,#8696,#8697),#13058);
#13250=SHAPE_REPRESENTATION('',(#7987,#8623,#8624,#8625,#8626,#8627,#8628,
#8629,#8630,#8631,#8632,#8633,#8634,#8635,#8636,#8637,#8638,#8639,#8640,
#8641,#8642,#8643,#8644,#8645,#8646,#8647,#8648,#8649,#8650,#8651,#8652,
#8653,#8654,#8655,#8656,#8657,#8658,#8659,#8660,#8661,#8662,#8663,#8664,
#8665,#8666,#8667,#8668,#8669,#8670,#8671,#8672,#8673,#8674,#8675,#8676,
#8677,#8678,#8679,#8680,#8681,#8682,#8683,#8684,#8685,#8686),#13059);
#13251=SHAPE_REPRESENTATION('',(#7988),#13060);
#13252=SHAPE_REPRESENTATION('',(#8007),#13061);
#13253=SHAPE_REPRESENTATION('',(#8030),#13062);
#13254=SHAPE_REPRESENTATION('',(#8037),#13063);
#13255=SHAPE_REPRESENTATION('',(#8044),#13064);
#13256=SHAPE_REPRESENTATION('',(#8051),#13065);
#13257=SHAPE_REPRESENTATION('',(#8064),#13066);
#13258=SHAPE_REPRESENTATION('',(#8077),#13067);
#13259=SHAPE_REPRESENTATION('',(#8095),#13068);
#13260=SHAPE_REPRESENTATION('',(#8113),#13069);
#13261=SHAPE_REPRESENTATION('',(#8131),#13070);
#13262=SHAPE_REPRESENTATION('',(#8149),#13071);
#13263=SHAPE_REPRESENTATION('',(#8160),#13072);
#13264=SHAPE_REPRESENTATION('',(#8171),#13073);
#13265=SHAPE_REPRESENTATION('',(#8202),#13074);
#13266=SHAPE_REPRESENTATION('',(#8217),#13075);
#13267=SHAPE_REPRESENTATION('',(#8234),#13076);
#13268=SHAPE_REPRESENTATION('',(#8251),#13077);
#13269=SHAPE_REPRESENTATION('',(#8261),#13078);
#13270=SHAPE_REPRESENTATION('',(#8271),#13079);
#13271=SHAPE_REPRESENTATION('',(#8321),#13080);
#13272=SHAPE_REPRESENTATION('',(#8347),#13081);
#13273=SHAPE_REPRESENTATION('',(#8390),#13082);
#13274=SHAPE_REPRESENTATION('',(#8411),#13083);
#13275=SHAPE_REPRESENTATION('',(#8422),#13084);
#13276=SHAPE_REPRESENTATION('',(#8450,#8687,#8688,#8689,#8690,#8691,#8692,
#8693,#8694,#8695),#13085);
#13277=SHAPE_REPRESENTATION('',(#8451),#13086);
#13278=SHAPE_REPRESENTATION('',(#8480),#13087);
#13279=SHAPE_REPRESENTATION('',(#8508,#8570,#8571,#8572),#13088);
#13280=SHAPE_REPRESENTATION('',(#8509),#13089);
#13281=SHAPE_REPRESENTATION('',(#8548),#13090);
#13282=SHAPE_REPRESENTATION('',(#8559),#13091);
#13283=SHAPE_REPRESENTATION('',(#8573),#13092);
#13284=SHAPE_REPRESENTATION('',(#8597),#13093);
#13285=PRODUCT_DEFINITION_CONTEXT('part definition',#13395,'design');
#13286=PRODUCT_DEFINITION('PAT-022','PAT-022',#13322,
#13285);
#13287=PRODUCT_DEFINITION('Chute and extrusion frame',
'Chute and extrusion frame',#13323,#13285);
#13288=PRODUCT_DEFINITION('Base','Base',#13324,#13285);
#13289=PRODUCT_DEFINITION('Top frame','Top frame',#13325,#13285);
#13290=PRODUCT_DEFINITION('Foot strip','Foot strip',#13326,#13285);
#13291=PRODUCT_DEFINITION('Foot strip (1)','Foot strip (1)',#13327,#13285);
#13292=PRODUCT_DEFINITION('Chute floor','Chute floor',#13328,#13285);
#13293=PRODUCT_DEFINITION('Chute side','Chute side',#13329,#13285);
#13294=PRODUCT_DEFINITION('Chute side (1)','Chute side (1)',#13330,#13285);
#13295=PRODUCT_DEFINITION('Chute support bracket',
'Chute support bracket',#13331,#13285);
#13296=PRODUCT_DEFINITION('Chute support bracket (1)',
'Chute support bracket (1)',#13332,#13285);
#13297=PRODUCT_DEFINITION('Chute support bracket (2)',
'Chute support bracket (2)',#13333,#13285);
#13298=PRODUCT_DEFINITION('Chute support bracket (3)',
'Chute support bracket (3)',#13334,#13285);
#13299=PRODUCT_DEFINITION('Outlet frame','Outlet frame',#13335,#13285);
#13300=PRODUCT_DEFINITION('Gate wiper gasket','Gate wiper gasket',#13336,
#13285);
#13301=PRODUCT_DEFINITION('Rail backing bar','Rail backing bar',#13337,
#13285);
#13302=PRODUCT_DEFINITION('Left gate guide','Left gate guide',#13338,#13285);
#13303=PRODUCT_DEFINITION('Gate guide bracket','Gate guide bracket',#13339,
#13285);
#13304=PRODUCT_DEFINITION('Gate guide bracket (1)',
'Gate guide bracket (1)',#13340,#13285);
#13305=PRODUCT_DEFINITION('Gate end stop','Gate end stop',#13341,#13285);
#13306=PRODUCT_DEFINITION('Gate end stop (1)','Gate end stop (1)',#13342,
#13285);
#13307=PRODUCT_DEFINITION('Slotted Extrusion - 20 x 20 x 400 mm',
'Slotted Extrusion - 20 x 20 x 400 mm',#13343,#13285);
#13308=PRODUCT_DEFINITION('Cap Screw - M5x20','Cap Screw - M5x20',#13344,
#13285);
#13309=PRODUCT_DEFINITION('Linear Guide Rail - 15 mm, 220 mm Long',
'Linear Guide Rail - 15 mm, 220 mm Long',#13345,#13285);
#13310=PRODUCT_DEFINITION('Captive slot nut','Captive slot nut',#13346,
#13285);
#13311=PRODUCT_DEFINITION('Flat Washer - M5','Flat Washer - M5',#13347,
#13285);
#13312=PRODUCT_DEFINITION('M5x30 frame screw','M5x30 frame screw',#13348,
#13285);
#13313=PRODUCT_DEFINITION('Gate and handle','Gate and handle',#13349,#13285);
#13314=PRODUCT_DEFINITION('Gate panel','Gate panel',#13350,#13285);
#13315=PRODUCT_DEFINITION('Gate grip','Gate grip',#13351,#13285);
#13316=PRODUCT_DEFINITION('Flanged Linear Guide Carriage - 15 mm',
'Flanged Linear Guide Carriage - 15 mm',#13352,#13285);
#13317=PRODUCT_DEFINITION('Block','Block',#13353,#13285);
#13318=PRODUCT_DEFINITION('End cap +','End cap +',#13354,#13285);
#13319=PRODUCT_DEFINITION('End cap','End cap',#13355,#13285);
#13320=PRODUCT_DEFINITION('M5x14 Cap Screw','M5x14 Cap Screw',#13356,#13285);
#13321=PRODUCT_DEFINITION('Cap Screw - M4x16','Cap Screw - M4x16',#13357,
#13285);
#13322=PRODUCT_DEFINITION_FORMATION('',$,#13397);
#13323=PRODUCT_DEFINITION_FORMATION('',$,#13398);
#13324=PRODUCT_DEFINITION_FORMATION('',$,#13399);
#13325=PRODUCT_DEFINITION_FORMATION('',$,#13400);
#13326=PRODUCT_DEFINITION_FORMATION('',$,#13401);
#13327=PRODUCT_DEFINITION_FORMATION('',$,#13402);
#13328=PRODUCT_DEFINITION_FORMATION('',$,#13403);
#13329=PRODUCT_DEFINITION_FORMATION('',$,#13404);
#13330=PRODUCT_DEFINITION_FORMATION('',$,#13405);
#13331=PRODUCT_DEFINITION_FORMATION('',$,#13406);
#13332=PRODUCT_DEFINITION_FORMATION('',$,#13407);
#13333=PRODUCT_DEFINITION_FORMATION('',$,#13408);
#13334=PRODUCT_DEFINITION_FORMATION('',$,#13409);
#13335=PRODUCT_DEFINITION_FORMATION('',$,#13410);
#13336=PRODUCT_DEFINITION_FORMATION('',$,#13411);
#13337=PRODUCT_DEFINITION_FORMATION('',$,#13412);
#13338=PRODUCT_DEFINITION_FORMATION('',$,#13413);
#13339=PRODUCT_DEFINITION_FORMATION('',$,#13414);
#13340=PRODUCT_DEFINITION_FORMATION('',$,#13415);
#13341=PRODUCT_DEFINITION_FORMATION('',$,#13416);
#13342=PRODUCT_DEFINITION_FORMATION('',$,#13417);
#13343=PRODUCT_DEFINITION_FORMATION('',$,#13418);
#13344=PRODUCT_DEFINITION_FORMATION('',$,#13419);
#13345=PRODUCT_DEFINITION_FORMATION('',$,#13420);
#13346=PRODUCT_DEFINITION_FORMATION('',$,#13421);
#13347=PRODUCT_DEFINITION_FORMATION('',$,#13422);
#13348=PRODUCT_DEFINITION_FORMATION('',$,#13423);
#13349=PRODUCT_DEFINITION_FORMATION('',$,#13424);
#13350=PRODUCT_DEFINITION_FORMATION('',$,#13425);
#13351=PRODUCT_DEFINITION_FORMATION('',$,#13426);
#13352=PRODUCT_DEFINITION_FORMATION('',$,#13427);
#13353=PRODUCT_DEFINITION_FORMATION('',$,#13428);
#13354=PRODUCT_DEFINITION_FORMATION('',$,#13429);
#13355=PRODUCT_DEFINITION_FORMATION('',$,#13430);
#13356=PRODUCT_DEFINITION_FORMATION('',$,#13431);
#13357=PRODUCT_DEFINITION_FORMATION('',$,#13432);
#13358=PRODUCT_RELATED_PRODUCT_CATEGORY('PAT-022','PAT-022',(#13397));
#13359=PRODUCT_RELATED_PRODUCT_CATEGORY('Chute and extrusion frame',
'Chute and extrusion frame',(#13398));
#13360=PRODUCT_RELATED_PRODUCT_CATEGORY('Base','Base',(#13399));
#13361=PRODUCT_RELATED_PRODUCT_CATEGORY('Top frame','Top frame',(#13400));
#13362=PRODUCT_RELATED_PRODUCT_CATEGORY('Foot strip','Foot strip',(#13401));
#13363=PRODUCT_RELATED_PRODUCT_CATEGORY('Foot strip (1)',
'Foot strip (1)',(#13402));
#13364=PRODUCT_RELATED_PRODUCT_CATEGORY('Chute floor','Chute floor',(#13403));
#13365=PRODUCT_RELATED_PRODUCT_CATEGORY('Chute side','Chute side',(#13404));
#13366=PRODUCT_RELATED_PRODUCT_CATEGORY('Chute side (1)',
'Chute side (1)',(#13405));
#13367=PRODUCT_RELATED_PRODUCT_CATEGORY('Chute support bracket',
'Chute support bracket',(#13406));
#13368=PRODUCT_RELATED_PRODUCT_CATEGORY('Chute support bracket (1)',
'Chute support bracket (1)',(#13407));
#13369=PRODUCT_RELATED_PRODUCT_CATEGORY('Chute support bracket (2)',
'Chute support bracket (2)',(#13408));
#13370=PRODUCT_RELATED_PRODUCT_CATEGORY('Chute support bracket (3)',
'Chute support bracket (3)',(#13409));
#13371=PRODUCT_RELATED_PRODUCT_CATEGORY('Outlet frame','Outlet frame',(#13410));
#13372=PRODUCT_RELATED_PRODUCT_CATEGORY('Gate wiper gasket',
'Gate wiper gasket',(#13411));
#13373=PRODUCT_RELATED_PRODUCT_CATEGORY('Rail backing bar',
'Rail backing bar',(#13412));
#13374=PRODUCT_RELATED_PRODUCT_CATEGORY('Left gate guide',
'Left gate guide',(#13413));
#13375=PRODUCT_RELATED_PRODUCT_CATEGORY('Gate guide bracket',
'Gate guide bracket',(#13414));
#13376=PRODUCT_RELATED_PRODUCT_CATEGORY('Gate guide bracket (1)',
'Gate guide bracket (1)',(#13415));
#13377=PRODUCT_RELATED_PRODUCT_CATEGORY('Gate end stop','Gate end stop',
(#13416));
#13378=PRODUCT_RELATED_PRODUCT_CATEGORY('Gate end stop (1)',
'Gate end stop (1)',(#13417));
#13379=PRODUCT_RELATED_PRODUCT_CATEGORY(
'Slotted Extrusion - 20 x 20 x 400 mm',
'Slotted Extrusion - 20 x 20 x 400 mm',(#13418));
#13380=PRODUCT_RELATED_PRODUCT_CATEGORY('Cap Screw - M5x20',
'Cap Screw - M5x20',(#13419));
#13381=PRODUCT_RELATED_PRODUCT_CATEGORY(
'Linear Guide Rail - 15 mm, 220 mm Long',
'Linear Guide Rail - 15 mm, 220 mm Long',(#13420));
#13382=PRODUCT_RELATED_PRODUCT_CATEGORY('Captive slot nut',
'Captive slot nut',(#13421));
#13383=PRODUCT_RELATED_PRODUCT_CATEGORY('Flat Washer - M5',
'Flat Washer - M5',(#13422));
#13384=PRODUCT_RELATED_PRODUCT_CATEGORY('M5x30 frame screw',
'M5x30 frame screw',(#13423));
#13385=PRODUCT_RELATED_PRODUCT_CATEGORY('Gate and handle',
'Gate and handle',(#13424));
#13386=PRODUCT_RELATED_PRODUCT_CATEGORY('Gate panel','Gate panel',(#13425));
#13387=PRODUCT_RELATED_PRODUCT_CATEGORY('Gate grip','Gate grip',(#13426));
#13388=PRODUCT_RELATED_PRODUCT_CATEGORY(
'Flanged Linear Guide Carriage - 15 mm',
'Flanged Linear Guide Carriage - 15 mm',(#13427));
#13389=PRODUCT_RELATED_PRODUCT_CATEGORY('Block','Block',(#13428));
#13390=PRODUCT_RELATED_PRODUCT_CATEGORY('End cap +','End cap +',(#13429));
#13391=PRODUCT_RELATED_PRODUCT_CATEGORY('End cap','End cap',(#13430));
#13392=PRODUCT_RELATED_PRODUCT_CATEGORY('M5x14 Cap Screw',
'M5x14 Cap Screw',(#13431));
#13393=PRODUCT_RELATED_PRODUCT_CATEGORY('Cap Screw - M4x16',
'Cap Screw - M4x16',(#13432));
#13394=APPLICATION_PROTOCOL_DEFINITION('international standard',
'automotive_design',2009,#13395);
#13395=APPLICATION_CONTEXT(
'Core Data for Automotive Mechanical Design Process');
#13396=PRODUCT_CONTEXT('part definition',#13395,'mechanical');
#13397=PRODUCT('PAT-022','PAT-022',
'PAT-022',(#13396));
#13398=PRODUCT('Chute and extrusion frame','Chute and extrusion frame',
'Chute and extrusion frame',(#13396));
#13399=PRODUCT('Base','Base','Base',(#13396));
#13400=PRODUCT('Top frame','Top frame','Top frame',(#13396));
#13401=PRODUCT('Foot strip','Foot strip','Foot strip',(#13396));
#13402=PRODUCT('Foot strip (1)','Foot strip (1)','Foot strip (1)',(#13396));
#13403=PRODUCT('Chute floor','Chute floor','Chute floor',(#13396));
#13404=PRODUCT('Chute side','Chute side','Chute side',(#13396));
#13405=PRODUCT('Chute side (1)','Chute side (1)','Chute side (1)',(#13396));
#13406=PRODUCT('Chute support bracket','Chute support bracket',
'Chute support bracket',(#13396));
#13407=PRODUCT('Chute support bracket (1)','Chute support bracket (1)',
'Chute support bracket (1)',(#13396));
#13408=PRODUCT('Chute support bracket (2)','Chute support bracket (2)',
'Chute support bracket (2)',(#13396));
#13409=PRODUCT('Chute support bracket (3)','Chute support bracket (3)',
'Chute support bracket (3)',(#13396));
#13410=PRODUCT('Outlet frame','Outlet frame','Outlet frame',(#13396));
#13411=PRODUCT('Gate wiper gasket','Gate wiper gasket',
'Gate wiper gasket',(#13396));
#13412=PRODUCT('Rail backing bar','Rail backing bar','Rail backing bar',
(#13396));
#13413=PRODUCT('Left gate guide','Left gate guide','Left gate guide',(#13396));
#13414=PRODUCT('Gate guide bracket','Gate guide bracket',
'Gate guide bracket',(#13396));
#13415=PRODUCT('Gate guide bracket (1)','Gate guide bracket (1)',
'Gate guide bracket (1)',(#13396));
#13416=PRODUCT('Gate end stop','Gate end stop','Gate end stop',(#13396));
#13417=PRODUCT('Gate end stop (1)','Gate end stop (1)','Gate end stop (1)',(#13396));
#13418=PRODUCT('Slotted Extrusion - 20 x 20 x 400 mm',
'Slotted Extrusion - 20 x 20 x 400 mm',
'Slotted Extrusion - 20 x 20 x 400 mm',(#13396));
#13419=PRODUCT('Cap Screw - M5x20','Cap Screw - M5x20',
'Cap Screw - M5x20',(#13396));
#13420=PRODUCT('Linear Guide Rail - 15 mm, 220 mm Long',
'Linear Guide Rail - 15 mm, 220 mm Long',
'Linear Guide Rail - 15 mm, 220 mm Long',(#13396));
#13421=PRODUCT('Captive slot nut','Captive slot nut','Captive slot nut',
(#13396));
#13422=PRODUCT('Flat Washer - M5','Flat Washer - M5','Flat Washer - M5',
(#13396));
#13423=PRODUCT('M5x30 frame screw','M5x30 frame screw',
'M5x30 frame screw',(#13396));
#13424=PRODUCT('Gate and handle','Gate and handle','Gate and handle',(#13396));
#13425=PRODUCT('Gate panel','Gate panel','Gate panel',(#13396));
#13426=PRODUCT('Gate grip','Gate grip','Gate grip',(#13396));
#13427=PRODUCT('Flanged Linear Guide Carriage - 15 mm',
'Flanged Linear Guide Carriage - 15 mm',
'Flanged Linear Guide Carriage - 15 mm',(#13396));
#13428=PRODUCT('Block','Block','Block',(#13396));
#13429=PRODUCT('End cap +','End cap +','End cap +',(#13396));
#13430=PRODUCT('End cap','End cap','End cap',(#13396));
#13431=PRODUCT('M5x14 Cap Screw','M5x14 Cap Screw','M5x14 Cap Screw',(#13396));
#13432=PRODUCT('Cap Screw - M4x16','Cap Screw - M4x16',
'Cap Screw - M4x16',(#13396));
#13433=PRESENTATION_STYLE_ASSIGNMENT((#13438));
#13434=PRESENTATION_STYLE_ASSIGNMENT((#13439));
#13435=PRESENTATION_STYLE_ASSIGNMENT((#13440));
#13436=PRESENTATION_STYLE_ASSIGNMENT((#13441));
#13437=PRESENTATION_STYLE_ASSIGNMENT((#13442));
#13438=SURFACE_STYLE_USAGE(.BOTH.,#13443);
#13439=SURFACE_STYLE_USAGE(.BOTH.,#13444);
#13440=SURFACE_STYLE_USAGE(.BOTH.,#13445);
#13441=SURFACE_STYLE_USAGE(.BOTH.,#13446);
#13442=SURFACE_STYLE_USAGE(.BOTH.,#13447);
#13443=SURFACE_SIDE_STYLE('',(#13448));
#13444=SURFACE_SIDE_STYLE('',(#13449));
#13445=SURFACE_SIDE_STYLE('',(#13450));
#13446=SURFACE_SIDE_STYLE('',(#13451));
#13447=SURFACE_SIDE_STYLE('',(#13452));
#13448=SURFACE_STYLE_FILL_AREA(#13453);
#13449=SURFACE_STYLE_FILL_AREA(#13454);
#13450=SURFACE_STYLE_FILL_AREA(#13455);
#13451=SURFACE_STYLE_FILL_AREA(#13456);
#13452=SURFACE_STYLE_FILL_AREA(#13457);
#13453=FILL_AREA_STYLE('Steel - Satin',(#13458));
#13454=FILL_AREA_STYLE('CAD Library Painted - Deep blue',(#13459));
#13455=FILL_AREA_STYLE('CAD Library Painted - Engineering blue',(#13460));
#13456=FILL_AREA_STYLE('CAD Library Painted - Steel gray',(#13461));
#13457=FILL_AREA_STYLE('CAD Library Painted - Graphite',(#13462));
#13458=FILL_AREA_STYLE_COLOUR('Steel - Satin',#13463);
#13459=FILL_AREA_STYLE_COLOUR('CAD Library Painted - Deep blue',#13464);
#13460=FILL_AREA_STYLE_COLOUR('CAD Library Painted - Engineering blue',
#13465);
#13461=FILL_AREA_STYLE_COLOUR('CAD Library Painted - Steel gray',#13466);
#13462=FILL_AREA_STYLE_COLOUR('CAD Library Painted - Graphite',#13467);
#13463=COLOUR_RGB('Steel - Satin',0.627450980392157,0.627450980392157,0.627450980392157);
#13464=COLOUR_RGB('CAD Library Painted - Deep blue',0.0784313725490196,
0.203921568627451,0.349019607843137);
#13465=COLOUR_RGB('CAD Library Painted - Engineering blue',0.12156862745098,
0.356862745098039,0.6);
#13466=COLOUR_RGB('CAD Library Painted - Steel gray',0.592156862745098,
0.631372549019608,0.67843137254902);
#13467=COLOUR_RGB('CAD Library Painted - Graphite',0.168627450980392,0.192156862745098,
0.231372549019608);
#13468=COLOUR_RGB('Dark Blue',0.08,0.2,0.34);
#13469=FILL_AREA_STYLE_COLOUR('',#13468);
#13470=FILL_AREA_STYLE('',(#13469));
#13471=SURFACE_STYLE_FILL_AREA(#13470);
#13472=SURFACE_SIDE_STYLE('',(#13471));
#13473=SURFACE_STYLE_USAGE(.BOTH.,#13472);
#13474=PRESENTATION_STYLE_ASSIGNMENT((#13473));
#13475=COLOUR_RGB('Light Blue',0.38,0.62,0.78);
#13476=FILL_AREA_STYLE_COLOUR('',#13475);
#13477=FILL_AREA_STYLE('',(#13476));
#13478=SURFACE_STYLE_FILL_AREA(#13477);
#13479=SURFACE_SIDE_STYLE('',(#13478));
#13480=SURFACE_STYLE_USAGE(.BOTH.,#13479);
#13481=PRESENTATION_STYLE_ASSIGNMENT((#13480));
#13482=COLOUR_RGB('Sky Blue',0.24,0.69,0.87);
#13483=FILL_AREA_STYLE_COLOUR('',#13482);
#13484=FILL_AREA_STYLE('',(#13483));
#13485=SURFACE_STYLE_FILL_AREA(#13484);
#13486=SURFACE_SIDE_STYLE('',(#13485));
#13487=SURFACE_STYLE_USAGE(.BOTH.,#13486);
#13488=PRESENTATION_STYLE_ASSIGNMENT((#13487));
#13489=COLOUR_RGB('Grey',0.48,0.52,0.57);
#13490=FILL_AREA_STYLE_COLOUR('',#13489);
#13491=FILL_AREA_STYLE('',(#13490));
#13492=SURFACE_STYLE_FILL_AREA(#13491);
#13493=SURFACE_SIDE_STYLE('',(#13492));
#13494=SURFACE_STYLE_USAGE(.BOTH.,#13493);
#13495=PRESENTATION_STYLE_ASSIGNMENT((#13494));
#13496=COLOUR_RGB('Black',0.12,0.14,0.17);
#13497=FILL_AREA_STYLE_COLOUR('',#13496);
#13498=FILL_AREA_STYLE('',(#13497));
#13499=SURFACE_STYLE_FILL_AREA(#13498);
#13500=SURFACE_SIDE_STYLE('',(#13499));
#13501=SURFACE_STYLE_USAGE(.BOTH.,#13500);
#13502=PRESENTATION_STYLE_ASSIGNMENT((#13501));
#13503=COLOUR_RGB('Off White',0.89,0.88,0.83);
#13504=FILL_AREA_STYLE_COLOUR('',#13503);
#13505=FILL_AREA_STYLE('',(#13504));
#13506=SURFACE_STYLE_FILL_AREA(#13505);
#13507=SURFACE_SIDE_STYLE('',(#13506));
#13508=SURFACE_STYLE_USAGE(.BOTH.,#13507);
#13509=PRESENTATION_STYLE_ASSIGNMENT((#13508));
ENDSEC;
END-ISO-10303-21;
